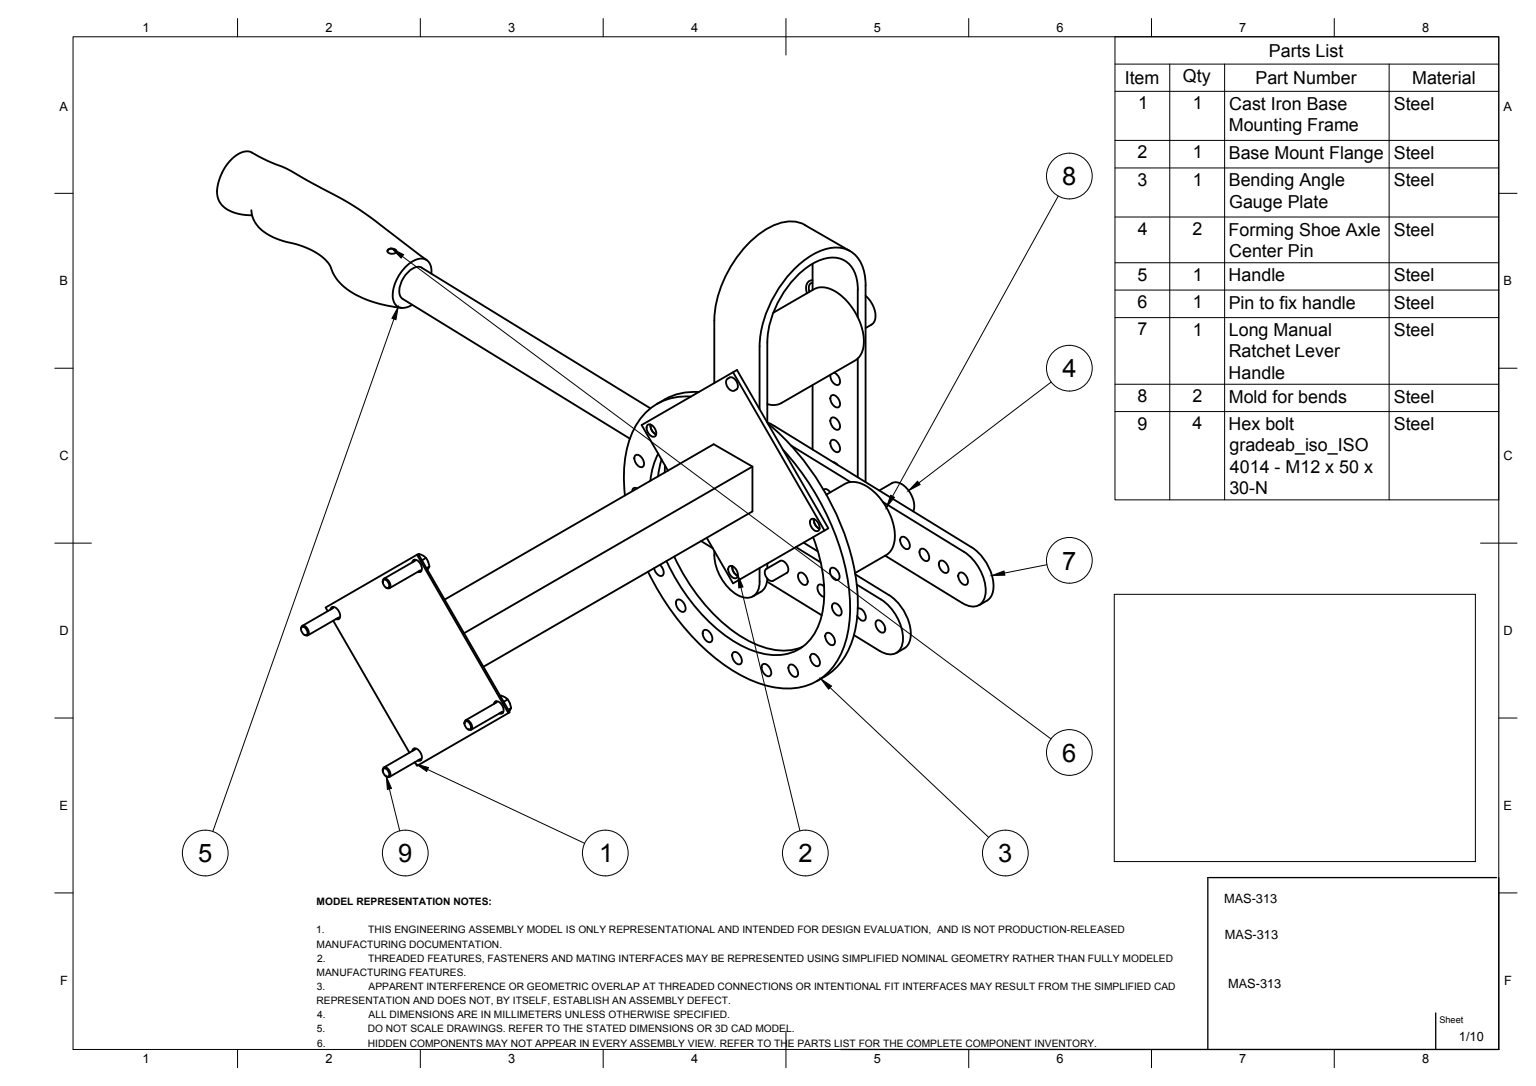
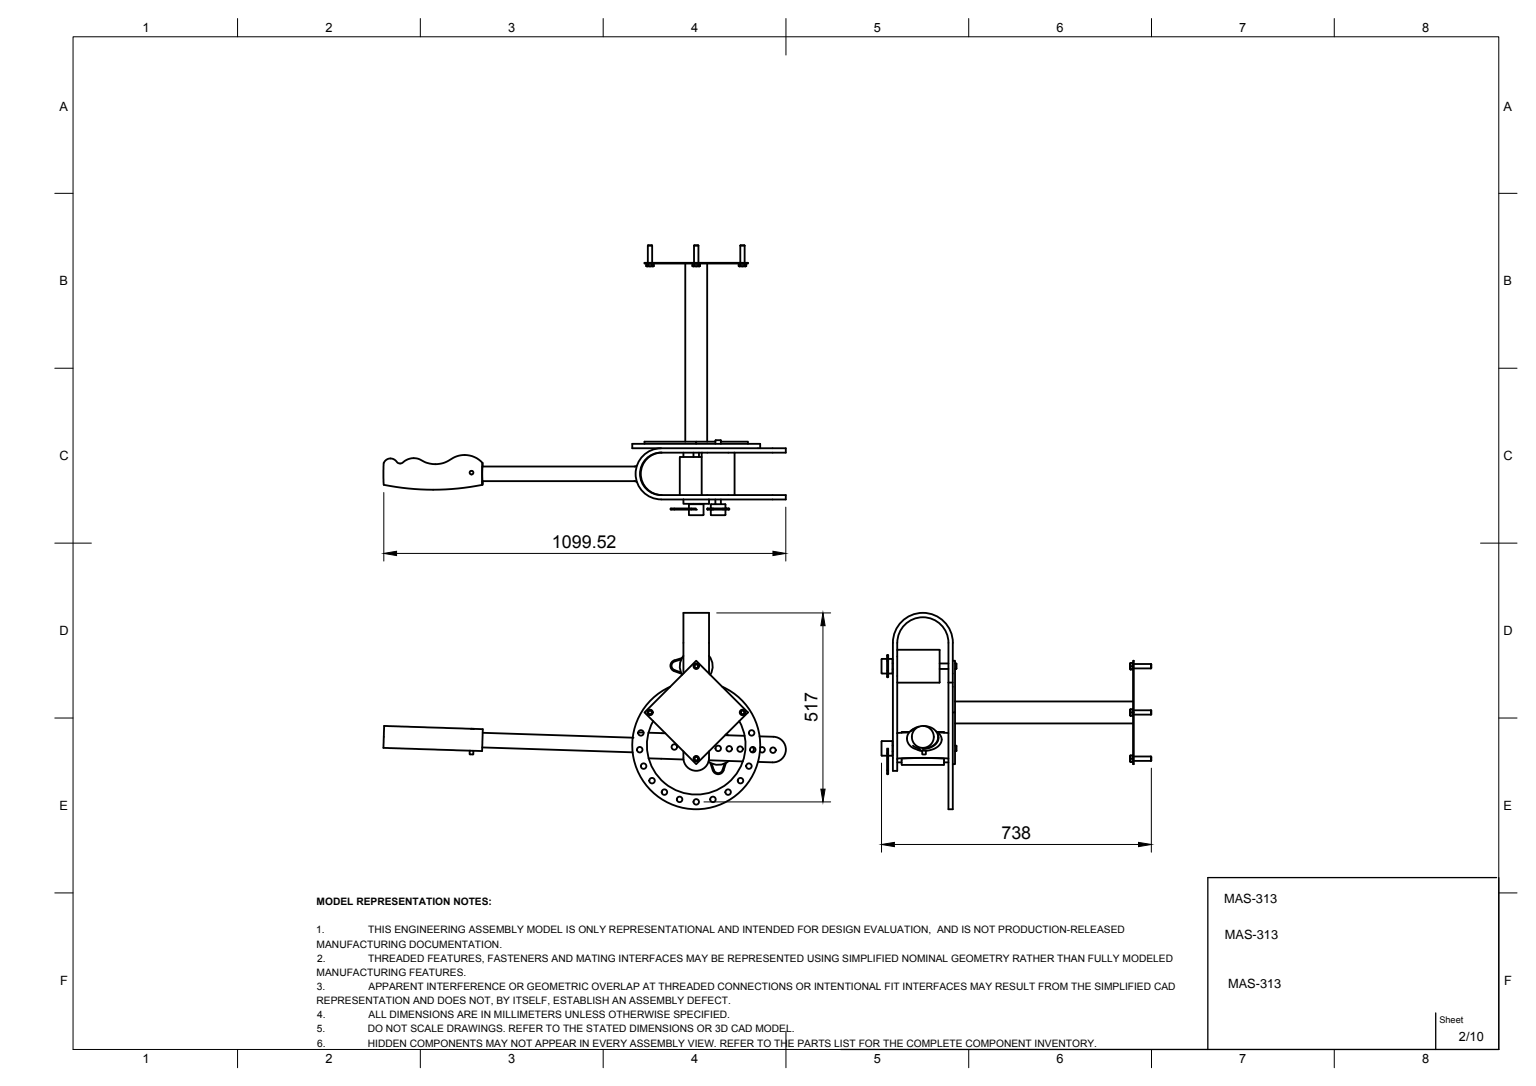
ISO-10303-21;
HEADER;
FILE_DESCRIPTION (('STEP AP214'),
    '1' );
FILE_NAME ('MAS-313',
    '2026-10-06T09:36:00',
    ( '' ),
    ( '' ),
    'SwSTEP 2.0',
    'SolidWorks 2025',
    '' );
FILE_SCHEMA (( 'AUTOMOTIVE_DESIGN' ));
ENDSEC;

DATA;
#1 = ORIENTED_EDGE ( 'NONE', *, *, #10134, .F. ) ;
#2 = ORIENTED_EDGE ( 'NONE', *, *, #7069, .T. ) ;
#3 = LINE ( 'NONE', #10333, #7200 ) ;
#4 = CARTESIAN_POINT ( 'NONE',  ( -828.8285638327245124, 78.34605190446923473, -105.0145692953451260 ) ) ;
#5 = EDGE_LOOP ( 'NONE', ( #11080, #1788 ) ) ;
#6 = CARTESIAN_POINT ( 'NONE',  ( -384.9774416452893888, 80.69083648313058177, -144.6406486762352870 ) ) ;
#7 = DIRECTION ( 'NONE',  ( 0.000000000000000000, 0.000000000000000000, 1.000000000000000000 ) ) ;
#8 = CARTESIAN_POINT ( 'NONE',  ( -374.9348459032029837, 78.20628728207141478, -105.0188168623670322 ) ) ;
#9 = CARTESIAN_POINT ( 'NONE',  ( -305.0000000000000568, 81.99999999999995737, -89.68077099980384048 ) ) ;
#10 = CIRCLE ( 'NONE', #8517, 8.500000000000007105 ) ;
#11 = EDGE_CURVE ( 'NONE', #3523, #3290, #9059, .T. ) ;
#12 = DIRECTION ( 'NONE',  ( -8.163404592832030268E-17, 1.000000000000000000, -0.000000000000000000 ) ) ;
#13 = CARTESIAN_POINT ( 'NONE',  ( -6.360897667028196044E-14, -494.9999999999998863, -141.4213562373094817 ) ) ;
#14 = EDGE_CURVE ( 'NONE', #10023, #7883, #9995, .T. ) ;
#15 = CARTESIAN_POINT ( 'NONE',  ( -795.0000000000070486, 70.44548139156158584, -96.78565065507937959 ) ) ;
#16 = CARTESIAN_POINT ( 'NONE',  ( -820.7717470982067880, 82.64484858469236883, -104.6903222377189593 ) ) ;
#17 = CYLINDRICAL_SURFACE ( 'NONE', #5203, 7.500000000000007105 ) ;
#18 = CIRCLE ( 'NONE', #8899, 134.9999999999999716 ) ;
#19 = CARTESIAN_POINT ( 'NONE',  ( -826.0529305544633871, 83.16438776978758085, -144.6472496521801929 ) ) ;
#20 = VERTEX_POINT ( 'NONE', #8026 ) ;
#21 = CARTESIAN_POINT ( 'NONE',  ( -824.1603064692799308, 83.67418067986842800, -144.6105757924095485 ) ) ;
#22 = ADVANCED_FACE ( 'NONE', ( #9876 ), #2276, .F. ) ;
#23 = SHAPE_DEFINITION_REPRESENTATION ( #9502, #690 ) ;
#24 = CARTESIAN_POINT ( 'NONE',  ( -374.1619648394964770, 92.84764663444484256, -97.33358173750130504 ) ) ;
#25 = ORIENTED_EDGE ( 'NONE', *, *, #6395, .T. ) ;
#26 = DIRECTION ( 'NONE',  ( 0.000000000000000000, 0.000000000000000000, 1.000000000000000000 ) ) ;
#27 = AXIS2_PLACEMENT_3D ( 'NONE', #9687, #6908, #2335 ) ;
#28 = CARTESIAN_POINT ( 'NONE',  ( -976.0610374937461984, 42.74778062430068104, -107.9061927053324155 ) ) ;
#29 = DIRECTION ( 'NONE',  ( 0.000000000000000000, 0.000000000000000000, 1.000000000000000000 ) ) ;
#30 = CARTESIAN_POINT ( 'NONE',  ( 19.97706055966621008, 179.9215598820742628, -126.1361639878079757 ) ) ;
#31 = CARTESIAN_POINT ( 'NONE',  ( 9.184850993605149917E-16, 0.000000000000000000, -133.9213562373095101 ) ) ;
#32 = TOROIDAL_SURFACE ( 'NONE', #418, 8.500000000000007105, 1.000000000000000000 ) ;
#33 = EDGE_CURVE ( 'NONE', #7221, #5849, #1766, .T. ) ;
#34 = ORIENTED_EDGE ( 'NONE', *, *, #7230, .T. ) ;
#35 = CARTESIAN_POINT ( 'NONE',  ( -374.8624431792070482, 77.47276654782569949, -154.2594059479313842 ) ) ;
#36 = CARTESIAN_POINT ( 'NONE',  ( -372.1683858186218004, 101.7385701426550071, -104.8071179324957569 ) ) ;
#37 = ORIENTED_EDGE ( 'NONE', *, *, #6606, .T. ) ;
#38 = CARTESIAN_POINT ( 'NONE',  ( -795.0000000000065938, 109.8950841424301217, -113.1262384684096105 ) ) ;
#39 = PRODUCT_RELATED_PRODUCT_CATEGORY ( 'part', '', ( #12175 ) ) ;
#40 = DIRECTION ( 'NONE',  ( -6.195440985631454085E-17, 0.000000000000000000, 1.000000000000000000 ) ) ;
#41 = CARTESIAN_POINT ( 'NONE',  ( -951.5459139781262365, 122.3346817490816676, -136.2353035311979852 ) ) ;
#42 = LINE ( 'NONE', #11363, #8844 ) ;
#43 = AXIS2_PLACEMENT_3D ( 'NONE', #1624, #5382, #1881 ) ;
#44 = CARTESIAN_POINT ( 'NONE',  ( -20.77482174596512010, 180.9926187296579201, -123.5402880645762451 ) ) ;
#45 = ORIENTED_EDGE ( 'NONE', *, *, #10615, .T. ) ;
#46 = DIRECTION ( 'NONE',  ( -0.7071067811865526798, 0.000000000000000000, 0.7071067811865423547 ) ) ;
#47 = EDGE_CURVE ( 'NONE', #6610, #12185, #4189, .T. ) ;
#48 = CARTESIAN_POINT ( 'NONE',  ( 7.653191805780027529E-16, 139.9999999999999716, -126.4213562373094959 ) ) ;
#49 = LINE ( 'NONE', #8712, #562 ) ;
#50 = CARTESIAN_POINT ( 'NONE',  ( -954.3284336448712111, 118.5422944683825932, -141.4553492942762318 ) ) ;
#51 = CARTESIAN_POINT ( 'NONE',  ( -379.1625717519825685, 101.9990905548760622, -123.9924296326342414 ) ) ;
#52 =( NAMED_UNIT ( * ) PLANE_ANGLE_UNIT ( ) SI_UNIT ( $, .RADIAN. ) );
#53 = DIRECTION ( 'NONE',  ( -8.163404592832030268E-17, 1.000000000000000000, -0.000000000000000000 ) ) ;
#54 = DIRECTION ( 'NONE',  ( -0.000000000000000000, 1.000000000000000000, 7.930164461608263644E-17 ) ) ;
#55 = ORIENTED_EDGE ( 'NONE', *, *, #5184, .F. ) ;
#56 = CARTESIAN_POINT ( 'NONE',  ( 1.561981751485805177E-12, 12.00000000000000000, 23.57864376269050410 ) ) ;
#57 = CARTESIAN_POINT ( 'NONE',  ( -370.6528479074003144, 106.2912024161782654, -136.2244394883228154 ) ) ;
#58 = ORIENTED_EDGE ( 'NONE', *, *, #10485, .F. ) ;
#59 = CARTESIAN_POINT ( 'NONE',  ( -1046.457602311632627, 98.67849639484583690, -149.7857175106632894 ) ) ;
#60 = CARTESIAN_POINT ( 'NONE',  ( -1054.407929976944160, 113.5897173251037628, -130.5712005305405228 ) ) ;
#61 = CIRCLE ( 'NONE', #6581, 7.500000000000007105 ) ;
#62 = FACE_BOUND ( 'NONE', #10137, .T. ) ;
#63 = ORIENTED_EDGE ( 'NONE', *, *, #11154, .T. ) ;
#64 = VERTEX_POINT ( 'NONE', #2451 ) ;
#65 = CARTESIAN_POINT ( 'NONE',  ( -365.0000000000000568, 81.99999999999997158, -124.6807709998038405 ) ) ;
#66 = CARTESIAN_POINT ( 'NONE',  ( -119.9999999999999858, 12.00000000000001421, -126.4213562373086575 ) ) ;
#67 = CARTESIAN_POINT ( 'NONE',  ( -1027.708477481189902, 65.70736702952426356, -149.7857175106639431 ) ) ;
#68 = EDGE_CURVE ( 'NONE', #11346, #11763, #11644, .T. ) ;
#69 = VERTEX_POINT ( 'NONE', #7089 ) ;
#70 = CARTESIAN_POINT ( 'NONE',  ( -384.9468357058332799, 80.02786880483864707, -144.5860799529720566 ) ) ;
#71 = CARTESIAN_POINT ( 'NONE',  ( 6.899999999999999467, -7.794228634059934713, 4.500000000000015987 ) ) ;
#72 = CARTESIAN_POINT ( 'NONE',  ( -374.8121035591796044, 76.80383275076532357, -95.25780428797004618 ) ) ;
#73 = LINE ( 'NONE', #6513, #3701 ) ;
#74 = AXIS2_PLACEMENT_3D ( 'NONE', #9091, #4403, #8176 ) ;
#75 = EDGE_LOOP ( 'NONE', ( #6909, #2744, #1662, #2481 ) ) ;
#76 = AXIS2_PLACEMENT_3D ( 'NONE', #1140, #8678, #11512 ) ;
#77 = DIRECTION ( 'NONE',  ( 0.000000000000000000, 0.000000000000000000, 1.000000000000000000 ) ) ;
#78 = CARTESIAN_POINT ( 'NONE',  ( 19.99739293773369653, 178.7258229095291426, -125.0390604444466902 ) ) ;
#79 = CARTESIAN_POINT ( 'NONE',  ( -1062.665377791213132, 57.01990411978262330, -103.3307627799634503 ) ) ;
#80 = CARTESIAN_POINT ( 'NONE',  ( -97.49999999999998579, 24.00000000000001421, -126.4213562373088564 ) ) ;
#81 = LINE ( 'NONE', #4059, #683 ) ;
#82 = CARTESIAN_POINT ( 'NONE',  ( -1032.658196452833636, 44.72920460984212809, -126.6442663926291914 ) ) ;
#83 = VERTEX_POINT ( 'NONE', #3428 ) ;
#84 = CARTESIAN_POINT ( 'NONE',  ( -384.0214413967224800, 73.66668219692796526, -106.4901515991773522 ) ) ;
#85 = ORIENTED_EDGE ( 'NONE', *, *, #1558, .T. ) ;
#86 = EDGE_CURVE ( 'NONE', #586, #9244, #5121, .T. ) ;
#87 = VECTOR ( 'NONE', #10625, 1000.000000000000000 ) ;
#88 = APPLICATION_PROTOCOL_DEFINITION ( 'draft international standard', 'automotive_design', 1998, #7796 ) ;
#89 = AXIS2_PLACEMENT_3D ( 'NONE', #10782, #5094, #8125 ) ;
#90 = VERTEX_POINT ( 'NONE', #4259 ) ;
#91 = CARTESIAN_POINT ( 'NONE',  ( -953.8433812051914629, 65.95343150956773570, -99.57582448894520155 ) ) ;
#92 = LINE ( 'NONE', #10358, #965 ) ;
#93 = EDGE_CURVE ( 'NONE', #7054, #9028, #4139, .T. ) ;
#94 = CYLINDRICAL_SURFACE ( 'NONE', #4643, 70.00000000000002842 ) ;
#95 = PRODUCT_DEFINITION_CONTEXT ( 'detailed design', #1716, 'design' ) ;
#96 = VECTOR ( 'NONE', #2050, 1000.000000000000000 ) ;
#97 = AXIS2_PLACEMENT_3D ( 'NONE', #11633, #3261, #1306 ) ;
#98 = CARTESIAN_POINT ( 'NONE',  ( -1054.691024341069351, 108.1159421897237110, -107.9061927053325149 ) ) ;
#99 = FACE_OUTER_BOUND ( 'NONE', #2484, .T. ) ;
#100 = CARTESIAN_POINT ( 'NONE',  ( -19.99217429592516737, 178.8549194765174946, -125.3522826812394584 ) ) ;
#101 = ORIENTED_EDGE ( 'NONE', *, *, #4439, .T. ) ;
#102 = CARTESIAN_POINT ( 'NONE',  ( -383.2436296729866285, 93.11778785828077787, -108.0524282450768681 ) ) ;
#103 = ORIENTED_EDGE ( 'NONE', *, *, #874, .T. ) ;
#105 = EDGE_CURVE ( 'NONE', #546, #9394, #11040, .T. ) ;
#104 = CARTESIAN_POINT ( 'NONE',  ( -1054.519145619997744, 111.4921997120089401, -113.1262384684101079 ) ) ;
#106 = CARTESIAN_POINT ( 'NONE',  ( 0.09252763182291999511, -8.674330214978049014, -2.975619346028157697 ) ) ;
#107 = CARTESIAN_POINT ( 'NONE',  ( -1024.848917040341576, 116.4131098345822437, -136.2353035311980420 ) ) ;
#108 = CARTESIAN_POINT ( 'NONE',  ( 19.97032670689476674, 177.8811654734197134, -125.7875625598146883 ) ) ;
#109 = CARTESIAN_POINT ( 'NONE',  ( -1045.884592419585942, 115.0579440276405450, -118.7903414690682524 ) ) ;
#110 = ORIENTED_EDGE ( 'NONE', *, *, #8930, .F. ) ;
#111 = DIRECTION ( 'NONE',  ( -8.163404592832030268E-17, 1.000000000000000000, -0.000000000000000000 ) ) ;
#112 = DIRECTION ( 'NONE',  ( 1.000000000000000000, 0.000000000000000000, 0.000000000000000000 ) ) ;
#113 = CARTESIAN_POINT ( 'NONE',  ( -954.7734463792789938, 107.7731650919854758, -149.7857175106632042 ) ) ;
#114 = LINE ( 'NONE', #2966, #2548 ) ;
#115 = DIRECTION ( 'NONE',  ( 0.000000000000000000, 1.000000000000000000, 0.000000000000000000 ) ) ;
#116 = ORIENTED_EDGE ( 'NONE', *, *, #6003, .T. ) ;
#117 = CYLINDRICAL_SURFACE ( 'NONE', #9034, 7.500000000000007105 ) ;
#118 = PRODUCT ( 'Base Mount Flange', 'Base Mount Flange', '', ( #4909 ) ) ;
#119 = CARTESIAN_POINT ( 'NONE',  ( -1065.000000000006366, 107.1049510380562850, -141.4553492942759192 ) ) ;
#120 = EDGE_CURVE ( 'NONE', #2594, #3971, #5709, .T. ) ;
#121 = EDGE_CURVE ( 'NONE', #609, #1988, #8932, .T. ) ;
#122 = ORIENTED_EDGE ( 'NONE', *, *, #10751, .T. ) ;
#123 = FACE_BOUND ( 'NONE', #7167, .T. ) ;
#124 = ORIENTED_EDGE ( 'NONE', *, *, #7991, .T. ) ;
#125 = VERTEX_POINT ( 'NONE', #4313 ) ;
#126 = CARTESIAN_POINT ( 'NONE',  ( 19.97657209060318806, 179.2792238463859746, -123.5006916350263282 ) ) ;
#127 = CARTESIAN_POINT ( 'NONE',  ( -21.00467209899894172, 181.7165653707129422, -124.9111601018296795 ) ) ;
#128 = FACE_BOUND ( 'NONE', #2869, .T. ) ;
#129 = CARTESIAN_POINT ( 'NONE',  ( -956.7203770923184720, 58.97922774997713447, -146.0307792196449839 ) ) ;
#130 = CARTESIAN_POINT ( 'NONE',  ( -383.8870708247850985, 73.11411249519194655, -142.6104777306848916 ) ) ;
#131 = CARTESIAN_POINT ( 'NONE',  ( -120.8820948793972434, 12.00000000000000000, -179.1989091883324363 ) ) ;
#132 = CARTESIAN_POINT ( 'NONE',  ( -384.9021618238296583, 79.34260306531722051, -104.8553288783483453 ) ) ;
#133 = VECTOR ( 'NONE', #10097, 1000.000000000000000 ) ;
#134 = CARTESIAN_POINT ( 'NONE',  ( 1.387778780781445676E-14, -58.00000000000000711, 126.4213562373094959 ) ) ;
#135 = ORIENTED_EDGE ( 'NONE', *, *, #8137, .F. ) ;
#136 = AXIS2_PLACEMENT_3D ( 'NONE', #2557, #579, #5269 ) ;
#137 = CARTESIAN_POINT ( 'NONE',  ( -818.1708872189576596, 40.82851623284144438, -103.3307627799635640 ) ) ;
#138 = CARTESIAN_POINT ( 'NONE',  ( -823.5000624989293101, 83.67424195610622917, -104.7509713550767287 ) ) ;
#139 = CARTESIAN_POINT ( 'NONE',  ( -901.8967518049312275, 57.00804855647886171, -130.5712005305400965 ) ) ;
#140 = VERTEX_POINT ( 'NONE', #3194 ) ;
#141 = CARTESIAN_POINT ( 'NONE',  ( -385.0078061158059768, 82.93686821115872476, -104.6668923901645769 ) ) ;
#142 = CARTESIAN_POINT ( 'NONE',  ( -825.4378685752795946, 73.92905737501402541, -154.6600603160834169 ) ) ;
#143 = EDGE_LOOP ( 'NONE', ( #3113, #5997, #4149, #12106, #10278, #5170, #6052 ) ) ;
#144 = SHAPE_DEFINITION_REPRESENTATION ( #1806, #1102 ) ;
#145 = ORIENTED_EDGE ( 'NONE', *, *, #5842, .F. ) ;
#146 = CARTESIAN_POINT ( 'NONE',  ( -1021.607260580486013, 54.24386729702176524, -118.7903414690683661 ) ) ;
#147 = VECTOR ( 'NONE', #6691, 1000.000000000000000 ) ;
#148 = DIRECTION ( 'NONE',  ( 0.000000000000000000, 0.000000000000000000, -1.000000000000000000 ) ) ;
#149 = FACE_OUTER_BOUND ( 'NONE', #6887, .T. ) ;
#150 = CIRCLE ( 'NONE', #8476, 7.500000000000007105 ) ;
#151 = CARTESIAN_POINT ( 'NONE',  ( -19.98114923013653765, 179.3963068953591176, -125.9321215961336975 ) ) ;
#152 = ORIENTED_EDGE ( 'NONE', *, *, #2859, .F. ) ;
#153 = CARTESIAN_POINT ( 'NONE',  ( -374.9443013845391874, 79.15238586648754904, -154.5107090977903113 ) ) ;
#154 = VERTEX_POINT ( 'NONE', #2390 ) ;
#155 = CARTESIAN_POINT ( 'NONE',  ( -954.3284336448667773, 118.5422944683823800, -107.9061927053323302 ) ) ;
#156 = AXIS2_PLACEMENT_3D ( 'NONE', #6549, #9206, #9335 ) ;
#157 = FACE_OUTER_BOUND ( 'NONE', #4978, .T. ) ;
#158 = CARTESIAN_POINT ( 'NONE',  ( -1054.519145619990923, 111.4921997120091106, -136.2353035311978999 ) ) ;
#159 = DIRECTION ( 'NONE',  ( -1.186840563529527301E-16, 1.000000000000000000, -0.000000000000000000 ) ) ;
#160 = AXIS2_PLACEMENT_3D ( 'NONE', #10271, #8167, #6559 ) ;
#161 = EDGE_CURVE ( 'NONE', #6627, #7697, #6700, .T. ) ;
#162 = CARTESIAN_POINT ( 'NONE',  ( -20.82968904857387216, 181.3053215700974192, -123.7910769712144798 ) ) ;
#163 = ORIENTED_EDGE ( 'NONE', *, *, #8870, .T. ) ;
#164 = CARTESIAN_POINT ( 'NONE',  ( -150.0000000000000000, -9.213203435596451385, -126.4213562373084301 ) ) ;
#165 = EDGE_CURVE ( 'NONE', #7498, #4712, #7501, .T. ) ;
#166 = AXIS2_PLACEMENT_3D ( 'NONE', #11994, #9209, #3384 ) ;
#167 = DIRECTION ( 'NONE',  ( 1.000000000000000000, -1.876626137810916309E-30, 2.081668171172161734E-17 ) ) ;
#168 = CYLINDRICAL_SURFACE ( 'NONE', #6692, 7.500000000000007105 ) ;
#169 = CARTESIAN_POINT ( 'NONE',  ( -852.9318753287220716, 113.3383058689776277, -141.4553492942764024 ) ) ;
#170 = CARTESIAN_POINT ( 'NONE',  ( -371.2169330467067994, 104.7056300760318379, -109.5948443055706036 ) ) ;
#171 = CARTESIAN_POINT ( 'NONE',  ( -126.4213562373094959, -492.9999999999998863, 2.255140518769849223E-14 ) ) ;
#172 = CARTESIAN_POINT ( 'NONE',  ( 1.414009460465297036E-14, -9.213203435596451385, -126.4213562373094959 ) ) ;
#173 = ORIENTED_EDGE ( 'NONE', *, *, #11290, .T. ) ;
#174 = CARTESIAN_POINT ( 'NONE',  ( -240.0000000000000000, 151.9999999999999716, -126.4213562373078190 ) ) ;
#175 = VECTOR ( 'NONE', #6548, 1000.000000000000000 ) ;
#176 = AXIS2_PLACEMENT_3D ( 'NONE', #10566, #11560, #2167 ) ;
#177 = FACE_BOUND ( 'NONE', #6264, .T. ) ;
#178 = VERTEX_POINT ( 'NONE', #3366 ) ;
#179 = ORIENTED_EDGE ( 'NONE', *, *, #161, .T. ) ;
#180 = CYLINDRICAL_SURFACE ( 'NONE', #1475, 20.00000000000004619 ) ;
#181 = CARTESIAN_POINT ( 'NONE',  ( -380.7070114274824846, 99.23877955377430737, -134.8374997946181111 ) ) ;
#182 = CARTESIAN_POINT ( 'NONE',  ( -956.4793285278399253, 64.87563161486532692, -149.7857175106635452 ) ) ;
#183 = EDGE_LOOP ( 'NONE', ( #1625, #2228, #7810, #4343, #5772, #11900, #7059 ) ) ;
#184 = ADVANCED_FACE ( 'NONE', ( #596 ), #4371, .T. ) ;
#185 = CARTESIAN_POINT ( 'NONE',  ( -384.7087986609971608, 86.59177257609081835, -144.1578396759514646 ) ) ;
#186 = CARTESIAN_POINT ( 'NONE',  ( 1.874378101782966050E-12, -6.000000000000006217, 61.07864376269051121 ) ) ;
#187 = CARTESIAN_POINT ( 'NONE',  ( -382.1259332444888628, 67.82440028630135487, -110.5571689112878033 ) ) ;
#188 = CARTESIAN_POINT ( 'NONE',  ( 0.000000000000000000, 0.000000000000000000, 0.000000000000000000 ) ) ;
#189 = ORIENTED_EDGE ( 'NONE', *, *, #1792, .T. ) ;
#190 = CARTESIAN_POINT ( 'NONE',  ( -954.4431216459919369, 51.77564274757662588, -136.2353035311985820 ) ) ;
#191 = PRODUCT_DEFINITION ( 'UNKNOWN', '', #10585, #95 ) ;
#192 = VERTEX_POINT ( 'NONE', #5981 ) ;
#193 = ORIENTED_EDGE ( 'NONE', *, *, #8592, .F. ) ;
#194 = CARTESIAN_POINT ( 'NONE',  ( -817.4144546772188278, 30.82543593413045713, -113.1262384684093689 ) ) ;
#195 = CARTESIAN_POINT ( 'NONE',  ( -822.2163178171820164, 83.41010758653678181, -104.7304854148475499 ) ) ;
#196 = LINE ( 'NONE', #11401, #4433 ) ;
#197 = EDGE_LOOP ( 'NONE', ( #6499, #7897, #12076, #5197 ) ) ;
#198 =( REPRESENTATION_RELATIONSHIP ('NONE','NONE', #12149, #4488 ) REPRESENTATION_RELATIONSHIP_WITH_TRANSFORMATION ( #4114 )SHAPE_REPRESENTATION_RELATIONSHIP( ) );
#199 = EDGE_CURVE ( 'NONE', #11915, #1856, #8826, .T. ) ;
#200 = CARTESIAN_POINT ( 'NONE',  ( -384.9575332945760806, 80.23676698716798228, -104.7563694268733059 ) ) ;
#201 = ORIENTED_EDGE ( 'NONE', *, *, #5756, .F. ) ;
#202 = CARTESIAN_POINT ( 'NONE',  ( -828.1602791247941013, 76.17169011767150266, -154.6744596958750151 ) ) ;
#203 = ORIENTED_EDGE ( 'NONE', *, *, #874, .F. ) ;
#204 = CARTESIAN_POINT ( 'NONE',  ( -305.0000000000000568, 11.99999999999998224, -89.68077099980384048 ) ) ;
#205 = APPLICATION_PROTOCOL_DEFINITION ( 'draft international standard', 'automotive_design', 1998, #366 ) ;
#206 = VERTEX_POINT ( 'NONE', #8210 ) ;
#207 = CARTESIAN_POINT ( 'NONE',  ( -1048.438004920983758, 39.66697241395321782, -122.7172756069793138 ) ) ;
#208 = DIRECTION ( 'NONE',  ( -0.000000000000000000, 1.000000000000000000, 7.930164461608263644E-17 ) ) ;
#209 = CARTESIAN_POINT ( 'NONE',  ( 0.1482032042081581624, 2.204400401829194056, -9.000000000000001776 ) ) ;
#210 = DIRECTION ( 'NONE',  ( 3.061276722312011504E-17, -1.000000000000000000, 0.000000000000000000 ) ) ;
#211 = CARTESIAN_POINT ( 'NONE',  ( -240.0000000000000000, 24.00000000000000711, -126.4213562373078190 ) ) ;
#212 = UNCERTAINTY_MEASURE_WITH_UNIT (LENGTH_MEASURE( 1.000000000000000082E-05 ), #7205, 'distance_accuracy_value', 'NONE');
#213 = VECTOR ( 'NONE', #11605, 1000.000000000000000 ) ;
#214 = CARTESIAN_POINT ( 'NONE',  ( -951.5459139781289650, 122.3346817490815681, -113.1262384684093263 ) ) ;
#215 = DIRECTION ( 'NONE',  ( -0.000000000000000000, 1.000000000000000000, 7.930164461608263644E-17 ) ) ;
#216 = DIRECTION ( 'NONE',  ( 0.000000000000000000, 0.000000000000000000, 1.000000000000000000 ) ) ;
#217 = ORIENTED_EDGE ( 'NONE', *, *, #11458, .T. ) ;
#218 = EDGE_LOOP ( 'NONE', ( #11467, #11457 ) ) ;
#219 = CARTESIAN_POINT ( 'NONE',  ( -1061.673215548682720, 86.58918783539685649, -95.06748246948023962 ) ) ;
#220 = CARTESIAN_POINT ( 'NONE',  ( -954.0688428831344936, 124.4732772249357282, -130.5712005305405796 ) ) ;
#221 = DIRECTION ( 'NONE',  ( -1.000000000000000000, 0.000000000000000000, 0.000000000000000000 ) ) ;
#222 = CARTESIAN_POINT ( 'NONE',  ( 19.92179295512113057, 178.7027072646551744, -122.9085123094865537 ) ) ;
#223 = CIRCLE ( 'NONE', #7140, 7.500000000000007105 ) ;
#224 = LINE ( 'NONE', #2033, #3608 ) ;
#225 = EDGE_LOOP ( 'NONE', ( #261, #5060, #2254, #7295, #1076, #408 ) ) ;
#226 = CYLINDRICAL_SURFACE ( 'NONE', #5194, 7.500000000000007105 ) ;
#227 = CARTESIAN_POINT ( 'NONE',  ( -820.5194676126008062, 82.43685310047841597, -104.6842045117117266 ) ) ;
#228 = CARTESIAN_POINT ( 'NONE',  ( 0.000000000000000000, -494.9999999999998863, 0.000000000000000000 ) ) ;
#229 = CARTESIAN_POINT ( 'NONE',  ( -1025.044148074459827, 113.2108726315406813, -141.4553492942762318 ) ) ;
#230 =( LENGTH_UNIT ( ) NAMED_UNIT ( * ) SI_UNIT ( .MILLI., .METRE. ) );
#231 = CARTESIAN_POINT ( 'NONE',  ( 120.8820948793965186, 0.000000000000000000, -194.1989091883332890 ) ) ;
#232 = FACE_BOUND ( 'NONE', #2861, .T. ) ;
#233 = VERTEX_POINT ( 'NONE', #6533 ) ;
#234 = CARTESIAN_POINT ( 'NONE',  ( -1010.922847972424620, 120.6260792194949829, -126.6442663926288503 ) ) ;
#235 = EDGE_CURVE ( 'NONE', #11998, #11124, #7336, .T. ) ;
#236 = DIRECTION ( 'NONE',  ( -0.000000000000000000, -1.000000000000000000, -1.757987137413040192E-14 ) ) ;
#237 = CARTESIAN_POINT ( 'NONE',  ( -853.1108559448500728, 99.60875591605696400, -149.7857175106632610 ) ) ;
#238 = EDGE_CURVE ( 'NONE', #2268, #7247, #10053, .T. ) ;
#239 = CARTESIAN_POINT ( 'NONE',  ( 0.000000000000000000, 0.000000000000000000, -89.68077099980401101 ) ) ;
#240 = ORIENTED_EDGE ( 'NONE', *, *, #4269, .F. ) ;
#241 = ORIENTED_EDGE ( 'NONE', *, *, #8867, .F. ) ;
#242 = CIRCLE ( 'NONE', #10114, 7.500000000000020428 ) ;
#243 = CARTESIAN_POINT ( 'NONE',  ( -383.7609474437092558, 91.40550212013970111, -142.3698073093449636 ) ) ;
#244 = CARTESIAN_POINT ( 'NONE',  ( 3.123963502971610252E-13, 12.00000000000000000, -96.42135623730949590 ) ) ;
#245 = CARTESIAN_POINT ( 'NONE',  ( -956.2104666674752025, 71.56905446038098262, -152.5758913445294809 ) ) ;
#246 = DIRECTION ( 'NONE',  ( 0.000000000000000000, 0.000000000000000000, -1.000000000000000000 ) ) ;
#247 = CARTESIAN_POINT ( 'NONE',  ( -384.0991065115986771, 74.01283611578425337, -143.0196247845297819 ) ) ;
#248 = FACE_OUTER_BOUND ( 'NONE', #11895, .T. ) ;
#249 = AXIS2_PLACEMENT_3D ( 'NONE', #6784, #11489, #10438 ) ;
#250 = EDGE_LOOP ( 'NONE', ( #6658, #11800 ) ) ;
#251 = CARTESIAN_POINT ( 'NONE',  ( -795.0000000000020464, 52.38665522077208436, -130.5712005305402670 ) ) ;
#252 = ORIENTED_EDGE ( 'NONE', *, *, #941, .T. ) ;
#253 = EDGE_CURVE ( 'NONE', #7231, #4288, #5520, .T. ) ;
#254 = FACE_OUTER_BOUND ( 'NONE', #3985, .T. ) ;
#255 = CARTESIAN_POINT ( 'NONE',  ( 20.99826841500651753, 178.6919330321067036, -124.8534679218782770 ) ) ;
#256 = VECTOR ( 'NONE', #4482, 1000.000000000000000 ) ;
#257 = CARTESIAN_POINT ( 'NONE',  ( -1014.004070199759440, 54.58258344709550869, -113.1262384684095537 ) ) ;
#258 = LINE ( 'NONE', #2469, #6072 ) ;
#259 = CARTESIAN_POINT ( 'NONE',  ( -1014.004070199769671, 54.58258344709567922, -136.2353035311988947 ) ) ;
#260 = EDGE_LOOP ( 'NONE', ( #3241, #8071, #5792, #1069 ) ) ;
#261 = ORIENTED_EDGE ( 'NONE', *, *, #5093, .F. ) ;
#262 = DIRECTION ( 'NONE',  ( 1.186840563529527301E-16, -1.000000000000000000, 0.000000000000000000 ) ) ;
#263 = ORIENTED_EDGE ( 'NONE', *, *, #5400, .T. ) ;
#264 = ORIENTED_EDGE ( 'NONE', *, *, #2535, .T. ) ;
#265 = CARTESIAN_POINT ( 'NONE',  ( -976.2351830775012331, 35.86345807843999012, -118.7903414690679824 ) ) ;
#266 = VECTOR ( 'NONE', #3751, 1000.000000000000000 ) ;
#267 = CIRCLE ( 'NONE', #6597, 5.035999999999999588 ) ;
#268 = CARTESIAN_POINT ( 'NONE',  ( -35.00000000000000000, 81.99999999999998579, 190.3192290001959748 ) ) ;
#269 = DIRECTION ( 'NONE',  ( 0.000000000000000000, 0.000000000000000000, -1.000000000000000000 ) ) ;
#270 = ADVANCED_FACE ( 'NONE', ( #2701 ), #10246, .F. ) ;
#271 = ADVANCED_FACE ( 'NONE', ( #9188 ), #1781, .F. ) ;
#272 = CARTESIAN_POINT ( 'NONE',  ( -1031.197907781702725, 107.2697845108577894, -103.3307627799635640 ) ) ;
#273 = DIRECTION ( 'NONE',  ( -0.000000000000000000, -0.000000000000000000, -1.000000000000000000 ) ) ;
#274 = CARTESIAN_POINT ( 'NONE',  ( -21.06063637301984670, 178.9270029669538360, -125.6999331669520501 ) ) ;
#275 = CIRCLE ( 'NONE', #3413, 1.000000000000001110 ) ;
#276 = VECTOR ( 'NONE', #8146, 1000.000000000000000 ) ;
#277 = ORIENTED_EDGE ( 'NONE', *, *, #5385, .T. ) ;
#278 = CIRCLE ( 'NONE', #3844, 7.500000000000013323 ) ;
#279 = DIRECTION ( 'NONE',  ( 1.000000000000000000, -1.262554838833776231E-16, 0.000000000000000000 ) ) ;
#280 = PRESENTATION_STYLE_ASSIGNMENT (( #11725 ) ) ;
#281 = ORIENTED_EDGE ( 'NONE', *, *, #1146, .T. ) ;
#282 = CARTESIAN_POINT ( 'NONE',  ( -853.3345817150102448, 81.97571759610518427, -95.06748246948041015 ) ) ;
#283 = EDGE_LOOP ( 'NONE', ( #6385, #2027 ) ) ;
#284 = CARTESIAN_POINT ( 'NONE',  ( -823.5047064235034213, 114.4566975831562274, -136.2353035311979284 ) ) ;
#285 = CARTESIAN_POINT ( 'NONE',  ( -6.106226635438360972E-13, 0.000000000000000000, -244.6807709998039400 ) ) ;
#286 =( BOUNDED_SURFACE ( )  B_SPLINE_SURFACE ( 3, 2, ( 
 ( #5085, #8801, #7187 ),
 ( #2485, #10957, #1263 ),
 ( #8857, #5024, #11650 ),
 ( #3170, #3727, #4408 ),
 ( #11016, #2547, #5517 ),
 ( #8178, #6322, #5324 ),
 ( #7317, #11945, #8318 ),
 ( #10089, #8249, #6509 ),
 ( #10030, #9093, #12007 ),
 ( #1688, #3526, #11218 ),
 ( #7251, #4472, #11082 ),
 ( #5581, #9355, #1623 ),
 ( #9160, #4606, #10151 ),
 ( #5381, #7377, #6262 ),
 ( #2741, #696, #632 ),
 ( #2607, #12145, #10219 ),
 ( #3462, #6382, #1561 ),
 ( #4667, #11150, #5445 ),
 ( #8445, #833, #9293 ),
 ( #9226, #767, #1818 ),
 ( #10279, #4542, #12077 ),
 ( #3587, #2673, #8382 ),
 ( #6448, #1756, #3659 ),
 ( #12203, #7433, #7499 ),
 ( #11272, #899, #10395 ),
 ( #1013, #1880, #10338 ),
 ( #9532, #6744, #8677 ),
 ( #2057, #5700, #5878 ),
 ( #7805, #8611, #130 ),
 ( #6810, #3848, #247 ),
 ( #5644, #3967, #9417 ),
 ( #1077, #4724, #2801 ),
 ( #8500, #5755, #10464 ),
 ( #4780, #6573, #7557 ),
 ( #9594, #5816, #8551 ),
 ( #2982, #6688, #4890 ),
 ( #953, #2119, #70 ),
 ( #1999, #7621, #6 ),
 ( #8730, #4035, #11511 ),
 ( #3782, #3908, #1938 ),
 ( #4834, #1139, #9657 ),
 ( #11329, #7682, #11389 ),
 ( #2928, #10521, #2870 ),
 ( #6630, #11451, #1198 ),
 ( #7737, #9474, #185 ),
 ( #10581, #3039, #4953 ),
 ( #11376, #2915, #12133 ),
 ( #2729, #1924, #3713 ),
 ( #5746, #7490, #5685 ),
 ( #6437, #6677, #10272 ),
 ( #11264, #5568, #10208 ),
 ( #9521, #1746, #2791 ),
 ( #8368, #11315, #11205 ),
 ( #3646, #5508, #1066 ),
 ( #9283, #5631, #1805 ),
 ( #6561, #1501, #821 ),
 ( #6498, #10325, #12064 ),
 ( #4766, #9405, #2854 ),
 ( #7611, #4713, #3773 ),
 ( #6620, #999, #8541 ),
 ( #57, #3836, #398 ),
 ( #9872, #8599, #11437 ) ),
 .UNSPECIFIED., .F., .F., .F. ) 
 B_SPLINE_SURFACE_WITH_KNOTS ( ( 4, 2, 2, 2, 2, 2, 2, 2, 2, 2, 2, 2, 2, 2, 2, 2, 2, 2, 2, 2, 2, 2, 2, 2, 2, 2, 2, 2, 2, 2, 4 ),
 ( 3, 3 ),
 ( 0.09449389133479987879, 0.1003997595432298551, 0.1063056277516598314, 0.1092585618558748195, 0.1107350289079823136, 0.1122114959600898076, 0.1181173641685197701, 0.1195938312206272502, 0.1210702982727347443, 0.1240232323769497325, 0.1269761664811647206, 0.1284526335332722147, 0.1299291005853797087, 0.1358349687938096850, 0.1387879028980246732, 0.1402643699501321672, 0.1417408370022396613, 0.1476467052106696376, 0.1491231722627771317, 0.1505996393148846257, 0.1535525734190996139, 0.1565055075233146020, 0.1594584416275295902, 0.1653643098359595387, 0.1683172439401744991, 0.1697937109922819932, 0.1712701780443894872, 0.1771760462528194635, 0.1801289803570344517, 0.1830819144612494398, 0.1889877826696794161 ),
 ( 0.000000000000000000, 1.000000000000000000 ),
 .UNSPECIFIED. ) 
 GEOMETRIC_REPRESENTATION_ITEM ( )  RATIONAL_B_SPLINE_SURFACE ( (
 ( 1.000000000000000000, 0.8172789612915526414, 1.000000000000000000),
 ( 1.000000000000000000, 0.8218272198189814359, 1.000000000000000000),
 ( 1.000000000000000000, 0.8252177520338900285, 1.000000000000000000),
 ( 1.000000000000000000, 0.8291640623197805704, 1.000000000000000000),
 ( 1.000000000000000000, 0.8296443862460527452, 1.000000000000000000),
 ( 1.000000000000000000, 0.8281763619574273871, 1.000000000000000000),
 ( 1.000000000000000000, 0.8273214979613470188, 1.000000000000000000),
 ( 1.000000000000000000, 0.8254906886306150327, 1.000000000000000000),
 ( 1.000000000000000000, 0.8247876722294519292, 1.000000000000000000),
 ( 1.000000000000000000, 0.8232192861295574149, 1.000000000000000000),
 ( 1.000000000000000000, 0.8223523569020266821, 1.000000000000000000),
 ( 1.000000000000000000, 0.8176244427683647675, 1.000000000000000000),
 ( 1.000000000000000000, 0.8125861978211987857, 1.000000000000000000),
 ( 1.000000000000000000, 0.8050068216217169947, 1.000000000000000000),
 ( 1.000000000000000000, 0.8034229420457332793, 1.000000000000000000),
 ( 1.000000000000000000, 0.8001526181735703069, 1.000000000000000000),
 ( 1.000000000000000000, 0.7984703186739749992, 1.000000000000000000),
 ( 1.000000000000000000, 0.7932997541396797914, 1.000000000000000000),
 ( 1.000000000000000000, 0.7896878191176920359, 1.000000000000000000),
 ( 1.000000000000000000, 0.7822263873999749650, 1.000000000000000000),
 ( 1.000000000000000000, 0.7783766572002538409, 1.000000000000000000),
 ( 1.000000000000000000, 0.7724948447777896243, 1.000000000000000000),
 ( 1.000000000000000000, 0.7705164146871855690, 1.000000000000000000),
 ( 1.000000000000000000, 0.7665366243600161278, 1.000000000000000000),
 ( 1.000000000000000000, 0.7645334732995007210, 1.000000000000000000),
 ( 1.000000000000000000, 0.7545994289160806723, 1.000000000000000000),
 ( 1.000000000000000000, 0.7468282588146691880, 1.000000000000000000),
 ( 1.000000000000000000, 0.7361158826353683127, 1.000000000000000000),
 ( 1.000000000000000000, 0.7327031703348744207, 1.000000000000000000),
 ( 1.000000000000000000, 0.7279177720675241714, 1.000000000000000000),
 ( 1.000000000000000000, 0.7263769756471946115, 1.000000000000000000),
 ( 1.000000000000000000, 0.7234575735669767083, 1.000000000000000000),
 ( 1.000000000000000000, 0.7220742453523991689, 1.000000000000000000),
 ( 1.000000000000000000, 0.7155655556167423992, 1.000000000000000000),
 ( 1.000000000000000000, 0.7116656400988581321, 1.000000000000000000),
 ( 1.000000000000000000, 0.7088249914908492100, 1.000000000000000000),
 ( 1.000000000000000000, 0.7083584775623817942, 1.000000000000000000),
 ( 1.000000000000000000, 0.7076383381209198076, 1.000000000000000000),
 ( 1.000000000000000000, 0.7073855737940044630, 1.000000000000000000),
 ( 1.000000000000000000, 0.7069609716970313151, 1.000000000000000000),
 ( 1.000000000000000000, 0.7071175024107954066, 1.000000000000000000),
 ( 1.000000000000000000, 0.7082797836801750790, 1.000000000000000000),
 ( 1.000000000000000000, 0.7092855318707916856, 1.000000000000000000),
 ( 1.000000000000000000, 0.7121081611133525113, 1.000000000000000000),
 ( 1.000000000000000000, 0.7139297788701386427, 1.000000000000000000),
 ( 1.000000000000000000, 0.7205123102341589592, 1.000000000000000000),
 ( 1.000000000000000000, 0.7262634879477153360, 1.000000000000000000),
 ( 1.000000000000000000, 0.7362377633225355433, 1.000000000000000000),
 ( 1.000000000000000000, 0.7397880641819555292, 1.000000000000000000),
 ( 1.000000000000000000, 0.7453704836958430224, 1.000000000000000000),
 ( 1.000000000000000000, 0.7472719429557758142, 1.000000000000000000),
 ( 1.000000000000000000, 0.7511059034608574825, 1.000000000000000000),
 ( 1.000000000000000000, 0.7530430930858292848, 1.000000000000000000),
 ( 1.000000000000000000, 0.7627925276597339321, 1.000000000000000000),
 ( 1.000000000000000000, 0.7707906794718482058, 1.000000000000000000),
 ( 1.000000000000000000, 0.7824407450661361452, 1.000000000000000000),
 ( 1.000000000000000000, 0.7862798113962640167, 1.000000000000000000),
 ( 1.000000000000000000, 0.7935920352645898790, 1.000000000000000000),
 ( 1.000000000000000000, 0.7970830763616314485, 1.000000000000000000),
 ( 1.000000000000000000, 0.8069453338637414541, 1.000000000000000000),
 ( 1.000000000000000000, 0.8127078027066928501, 1.000000000000000000),
 ( 1.000000000000000000, 0.8173438319342977154, 1.000000000000000000) ) ) 
 REPRESENTATION_ITEM ( '' )  SURFACE ( )  );
#287 = CIRCLE ( 'NONE', #5208, 7.500000000000007105 ) ;
#288 = AXIS2_PLACEMENT_3D ( 'NONE', #7289, #5491, #4381 ) ;
#289 = ORIENTED_EDGE ( 'NONE', *, *, #5265, .F. ) ;
#290 = CARTESIAN_POINT ( 'NONE',  ( -821.1548363108382773, 74.44610204637874062, -143.1996371447159788 ) ) ;
#291 = PLANE ( 'NONE',  #9364 ) ;
#292 = CARTESIAN_POINT ( 'NONE',  ( -13.32222501832919193, 180.2041921146325762, -184.1652315311841051 ) ) ;
#293 = CARTESIAN_POINT ( 'NONE',  ( -1037.392967692951970, 114.2240391150264998, -136.2353035311982126 ) ) ;
#294 = CARTESIAN_POINT ( 'NONE',  ( -372.7969387542311210, 100.6399613739977497, -117.3710749709770198 ) ) ;
#295 = CARTESIAN_POINT ( 'NONE',  ( -7.499999999999979572, -6.999999999999979572, -124.6807709998038405 ) ) ;
#296 = AXIS2_PLACEMENT_3D ( 'NONE', #7544, #3832, #1922 ) ;
#297 = FACE_BOUND ( 'NONE', #8922, .T. ) ;
#298 = ORIENTED_EDGE ( 'NONE', *, *, #7352, .T. ) ;
#299 = CARTESIAN_POINT ( 'NONE',  ( 3.123963502971610252E-13, 164.0000000000000000, -96.42135623730948168 ) ) ;
#300 = CARTESIAN_POINT ( 'NONE',  ( -1060.756016675586807, 112.8516620848305934, -124.6807709998040821 ) ) ;
#301 = CARTESIAN_POINT ( 'NONE',  ( 7.500000000000022204, -9.213203435596451385, -126.4213562373094959 ) ) ;
#302 = CARTESIAN_POINT ( 'NONE',  ( -1037.550865396555764, 105.7975851359348667, -146.0307792196445860 ) ) ;
#303 = DIRECTION ( 'NONE',  ( -1.186840563529527301E-16, 1.000000000000000000, -0.000000000000000000 ) ) ;
#304 = ORIENTED_EDGE ( 'NONE', *, *, #9166, .F. ) ;
#305 = AXIS2_PLACEMENT_3D ( 'NONE', #12094, #1705, #10105 ) ;
#306 = EDGE_LOOP ( 'NONE', ( #4987, #12037, #7872, #11168 ) ) ;
#307 = EDGE_CURVE ( 'NONE', #1954, #154, #9065, .T. ) ;
#308 = FACE_BOUND ( 'NONE', #6793, .T. ) ;
#309 = CARTESIAN_POINT ( 'NONE',  ( -953.8433812051875975, 65.95343150956774991, -149.7857175106634315 ) ) ;
#310 = CARTESIAN_POINT ( 'NONE',  ( -823.8285638327238303, 78.67432280806536937, -89.68077099980398259 ) ) ;
#311 = DIRECTION ( 'NONE',  ( -1.000000000000000000, 0.000000000000000000, 0.000000000000000000 ) ) ;
#312 = DIRECTION ( 'NONE',  ( -1.000000000000000000, 0.000000000000000000, 0.000000000000000000 ) ) ;
#313 = CARTESIAN_POINT ( 'NONE',  ( -854.0803342822151762, 23.97549884981696167, -130.5712005305403238 ) ) ;
#314 = AXIS2_PLACEMENT_3D ( 'NONE', #7746, #6638, #6880 ) ;
#315 = ORIENTED_EDGE ( 'NONE', *, *, #3330, .T. ) ;
#316 = EDGE_LOOP ( 'NONE', ( #9146, #634 ) ) ;
#317 = CARTESIAN_POINT ( 'NONE',  ( -1028.454949082212806, 53.01113643315385104, -113.1262384684094400 ) ) ;
#318 = DIRECTION ( 'NONE',  ( -3.061276722312011504E-17, 1.000000000000000000, 0.000000000000000000 ) ) ;
#319 = CARTESIAN_POINT ( 'NONE',  ( 45.53315400109643463, 12.00000000000000000, -230.3419396193597208 ) ) ;
#320 = CARTESIAN_POINT ( 'NONE',  ( -1038.664246639927342, 43.28664065472985811, -136.2353035311990084 ) ) ;
#321 = EDGE_CURVE ( 'NONE', #10730, #10836, #6230, .T. ) ;
#322 = ORIENTED_EDGE ( 'NONE', *, *, #4849, .T. ) ;
#323 = CYLINDRICAL_SURFACE ( 'NONE', #3336, 7.500000000000007105 ) ;
#324 = CARTESIAN_POINT ( 'NONE',  ( -380.4203626278499542, 64.21146706504150359, -115.5204214313296376 ) ) ;
#325 = ORIENTED_EDGE ( 'NONE', *, *, #5571, .T. ) ;
#326 = CARTESIAN_POINT ( 'NONE',  ( -824.4849247483655290, 73.70682285379986354, -154.6506428397234743 ) ) ;
#327 = ORIENTED_EDGE ( 'NONE', *, *, #355, .T. ) ;
#328 = EDGE_LOOP ( 'NONE', ( #135, #8709, #7075, #7838 ) ) ;
#329 = CARTESIAN_POINT ( 'NONE',  ( -1065.000000000003865, 52.00000000000021316, -126.6442663926290493 ) ) ;
#330 = DIRECTION ( 'NONE',  ( -1.000000000000000000, 0.000000000000000000, 0.000000000000000000 ) ) ;
#331 = DIRECTION ( 'NONE',  ( 1.000000000000000000, 0.000000000000000000, 1.224646799147353207E-16 ) ) ;
#332 = AXIS2_PLACEMENT_3D ( 'NONE', #843, #8325, #8259 ) ;
#333 = DIRECTION ( 'NONE',  ( 0.000000000000000000, -1.156482317317870246E-16, 1.000000000000000000 ) ) ;
#334 = CIRCLE ( 'NONE', #5074, 57.99999999999999289 ) ;
#335 = CARTESIAN_POINT ( 'NONE',  ( -1061.468168685228193, 92.73456844357777129, -96.78565065507918064 ) ) ;
#336 = LINE ( 'NONE', #1445, #8050 ) ;
#337 = CARTESIAN_POINT ( 'NONE',  ( 19.00000000000000000, 197.0000000000000000, -124.6807709998038405 ) ) ;
#338 = VERTEX_POINT ( 'NONE', #2508 ) ;
#339 = LINE ( 'NONE', #9047, #1075 ) ;
#340 = EDGE_CURVE ( 'NONE', #2669, #5042, #5605, .T. ) ;
#341 = CIRCLE ( 'NONE', #6268, 30.00000000000021316 ) ;
#342 = EDGE_CURVE ( 'NONE', #12110, #8166, #11773, .T. ) ;
#343 =( NAMED_UNIT ( * ) PLANE_ANGLE_UNIT ( ) SI_UNIT ( $, .RADIAN. ) );
#344 = EDGE_LOOP ( 'NONE', ( #2553, #10547, #8461, #7126 ) ) ;
#345 = CARTESIAN_POINT ( 'NONE',  ( -1055.782959745578182, 85.17781532426863578, -95.06748246948041015 ) ) ;
#346 = EDGE_LOOP ( 'NONE', ( #11443, #5040 ) ) ;
#347 = CARTESIAN_POINT ( 'NONE',  ( -1021.743962174751232, 119.2557508373789403, -124.6807709998040110 ) ) ;
#348 = CARTESIAN_POINT ( 'NONE',  ( 154.5043356068769071, 12.00000000000000000, -109.5666613060171670 ) ) ;
#349 = EDGE_CURVE ( 'NONE', #7831, #3787, #3152, .T. ) ;
#350 = CARTESIAN_POINT ( 'NONE',  ( 151.3258811035896656, 12.00000000000000000, -48.63263083939796871 ) ) ;
#351 = AXIS2_PLACEMENT_3D ( 'NONE', #10311, #1910, #9449 ) ;
#352 = DIRECTION ( 'NONE',  ( 0.000000000000000000, 0.000000000000000000, 1.000000000000000000 ) ) ;
#353 = DIRECTION ( 'NONE',  ( -0.000000000000000000, -1.000000000000000000, 0.000000000000000000 ) ) ;
#354 = CARTESIAN_POINT ( 'NONE',  ( -1048.438004920983303, 39.66697241395321782, -124.6807709998044800 ) ) ;
#355 = EDGE_CURVE ( 'NONE', #1262, #3617, #2145, .T. ) ;
#356 = DIRECTION ( 'NONE',  ( 0.000000000000000000, -1.000000000000000000, -7.930164461608263644E-17 ) ) ;
#357 = CIRCLE ( 'NONE', #7273, 7.499999999999992895 ) ;
#358 = ORIENTED_EDGE ( 'NONE', *, *, #9645, .T. ) ;
#359 = FACE_OUTER_BOUND ( 'NONE', #1203, .T. ) ;
#360 = PLANE ( 'NONE',  #530 ) ;
#361 = CARTESIAN_POINT ( 'NONE',  ( -1024.691966601151762, 118.8493250655917564, -126.6442663926291061 ) ) ;
#362 = AXIS2_PLACEMENT_3D ( 'NONE', #5126, #8886, #3258 ) ;
#363 = CARTESIAN_POINT ( 'NONE',  ( -375.0000000000000000, 81.99999999999995737, -89.68077099980384048 ) ) ;
#364 = CARTESIAN_POINT ( 'NONE',  ( -374.9435208796285224, 79.09557628031252818, -94.85325544560421918 ) ) ;
#365 = ORIENTED_EDGE ( 'NONE', *, *, #10686, .T. ) ;
#366 = APPLICATION_CONTEXT ( 'automotive_design' ) ;
#367 = CIRCLE ( 'NONE', #4729, 7.500000000000007105 ) ;
#368 = VERTEX_POINT ( 'NONE', #31 ) ;
#369 = CARTESIAN_POINT ( 'NONE',  ( -90.00000000000000000, 152.0000000000000000, -126.4213562373088564 ) ) ;
#370 = FACE_BOUND ( 'NONE', #3925, .T. ) ;
#371 = CIRCLE ( 'NONE', #8725, 7.500000000000007105 ) ;
#372 = DIRECTION ( 'NONE',  ( 0.000000000000000000, -1.000000000000000000, -1.850371707708592551E-14 ) ) ;
#373 = CARTESIAN_POINT ( 'NONE',  ( -22.49999999999997868, -9.213203435596451385, -126.4213562373092685 ) ) ;
#374 = CARTESIAN_POINT ( 'NONE',  ( -827.5978224575839022, 75.37295367873073815, -94.68020981275554959 ) ) ;
#375 =( NAMED_UNIT ( * ) SI_UNIT ( $, .STERADIAN. ) SOLID_ANGLE_UNIT ( ) );
#376 = CIRCLE ( 'NONE', #5908, 7.500000000000012434 ) ;
#377 = EDGE_LOOP ( 'NONE', ( #4540, #1681, #1210, #5686, #11186, #2942, #6085, #5745, #3833, #8762 ) ) ;
#378 = CARTESIAN_POINT ( 'NONE',  ( -1062.923339974281134, 49.86928741160674150, -136.2353035311989515 ) ) ;
#379 = ORIENTED_EDGE ( 'NONE', *, *, #11461, .F. ) ;
#380 = ORIENTED_EDGE ( 'NONE', *, *, #161, .F. ) ;
#381 = DIRECTION ( 'NONE',  ( -0.000000000000000000, 1.000000000000000000, -0.000000000000000000 ) ) ;
#382 = CARTESIAN_POINT ( 'NONE',  ( -1017.158871447982051, 53.64146012065780411, -122.7172756069791717 ) ) ;
#383 = EDGE_LOOP ( 'NONE', ( #2203, #8907 ) ) ;
#384 = CARTESIAN_POINT ( 'NONE',  ( -151.3258811035894098, 12.00000000000000000, -48.63263083939678921 ) ) ;
#385 = CARTESIAN_POINT ( 'NONE',  ( -822.5313098515729280, 73.83434793536794416, -154.6477719089843390 ) ) ;
#386 = ORIENTED_EDGE ( 'NONE', *, *, #9875, .T. ) ;
#387 = ORIENTED_EDGE ( 'NONE', *, *, #9652, .F. ) ;
#388 = CARTESIAN_POINT ( 'NONE',  ( -976.2517683711888594, 35.25052392388814582, -122.7172756069790296 ) ) ;
#389 = EDGE_CURVE ( 'NONE', #4400, #11584, #1104, .T. ) ;
#390 = DIRECTION ( 'NONE',  ( 0.000000000000000000, 0.000000000000000000, -1.000000000000000000 ) ) ;
#391 = EDGE_CURVE ( 'NONE', #7319, #11283, #7095, .T. ) ;
#392 = CARTESIAN_POINT ( 'NONE',  ( 0.07661102881317549684, 6.914460432017338398, 6.023803224821312696 ) ) ;
#393 = CARTESIAN_POINT ( 'NONE',  ( -1025.928429817214464, 97.79385104913474436, -96.78565065507955012 ) ) ;
#394 = CYLINDRICAL_SURFACE ( 'NONE', #10869, 134.9999999999999716 ) ;
#395 = ORIENTED_EDGE ( 'NONE', *, *, #7971, .T. ) ;
#396 = ORIENTED_EDGE ( 'NONE', *, *, #11359, .T. ) ;
#397 = CARTESIAN_POINT ( 'NONE',  ( -795.0000000000002274, 98.77454568802498613, -99.57582448894500260 ) ) ;
#398 = CARTESIAN_POINT ( 'NONE',  ( -380.0318359341034693, 100.5075656702939142, -132.3766003259852084 ) ) ;
#399 = CARTESIAN_POINT ( 'NONE',  ( -951.4198147059589701, 125.0824040815807194, -124.6807709998040252 ) ) ;
#400 = CYLINDRICAL_SURFACE ( 'NONE', #7484, 7.500000000000007105 ) ;
#401 = EDGE_CURVE ( 'NONE', #10520, #8134, #578, .T. ) ;
#402 = CARTESIAN_POINT ( 'NONE',  ( -180.0000000000000000, 12.00000000000001421, -126.4213562373082453 ) ) ;
#403 = EDGE_CURVE ( 'NONE', #4980, #6173, #8091, .T. ) ;
#404 = FACE_BOUND ( 'NONE', #5340, .T. ) ;
#405 = CARTESIAN_POINT ( 'NONE',  ( 126.4213562373094959, -6.000000000000000000, -6.938893903907228378E-15 ) ) ;
#406 = PRODUCT_DEFINITION ( 'UNKNOWN', '', #11578, #8636 ) ;
#407 = FACE_OUTER_BOUND ( 'NONE', #12097, .T. ) ;
#408 = ORIENTED_EDGE ( 'NONE', *, *, #9663, .F. ) ;
#409 = CARTESIAN_POINT ( 'NONE',  ( 1.874378101782966050E-12, 152.0000000000000000, 53.57864376269051832 ) ) ;
#410 = CARTESIAN_POINT ( 'NONE',  ( -1017.810720698608179, 119.7719591276206046, -126.6442663926290493 ) ) ;
#411 = DIRECTION ( 'NONE',  ( -0.000000000000000000, -1.000000000000000000, -0.000000000000000000 ) ) ;
#412 = AXIS2_PLACEMENT_3D ( 'NONE', #9186, #721, #4497 ) ;
#413 = CARTESIAN_POINT ( 'NONE',  ( 1.387778780781445676E-14, -494.9999999999998863, 126.4213562373094959 ) ) ;
#414 = EDGE_CURVE ( 'NONE', #957, #11231, #4747, .T. ) ;
#415 = ORIENTED_EDGE ( 'NONE', *, *, #2463, .T. ) ;
#416 = CARTESIAN_POINT ( 'NONE',  ( 19.96510381999703654, 179.6655525025668680, -123.2864411696423019 ) ) ;
#417 = DIRECTION ( 'NONE',  ( 2.081668171172161734E-17, 4.930380657631307143E-31, -1.000000000000000000 ) ) ;
#418 = AXIS2_PLACEMENT_3D ( 'NONE', #4659, #2540, #5635 ) ;
#419 = CARTESIAN_POINT ( 'NONE',  ( -373.3204616456844747, 97.25197993938448349, -149.1095482086399784 ) ) ;
#420 = DIRECTION ( 'NONE',  ( -0.000000000000000000, 1.000000000000000000, 0.000000000000000000 ) ) ;
#421 = DIRECTION ( 'NONE',  ( 0.000000000000000000, -1.189524669241239115E-16, 1.000000000000000000 ) ) ;
#422 = LINE ( 'NONE', #11515, #6475 ) ;
#423 = AXIS2_PLACEMENT_3D ( 'NONE', #2783, #4705, #7030 ) ;
#424 = EDGE_LOOP ( 'NONE', ( #6274, #101, #7246, #3774 ) ) ;
#425 = CARTESIAN_POINT ( 'NONE',  ( -901.9718911164696920, 59.00785292138922244, -136.2353035311984115 ) ) ;
#426 = APPLICATION_CONTEXT ( 'automotive_design' ) ;
#427 = VECTOR ( 'NONE', #2802, 999.9999999999998863 ) ;
#428 = ORIENTED_EDGE ( 'NONE', *, *, #8066, .T. ) ;
#429 = CARTESIAN_POINT ( 'NONE',  ( 30.00000000000000000, -492.9999999999998863, -30.00000000000000000 ) ) ;
#430 = CARTESIAN_POINT ( 'NONE',  ( -1062.996098538733122, 47.98024286075321498, -118.7903414690683377 ) ) ;
#431 = DIRECTION ( 'NONE',  ( 0.000000000000000000, 0.000000000000000000, 1.000000000000000000 ) ) ;
#432 = CARTESIAN_POINT ( 'NONE',  ( -824.1522960622456822, 83.67452213711085562, -95.25851046848316628 ) ) ;
#433 = CARTESIAN_POINT ( 'NONE',  ( -818.8285638327243987, 78.67432280806558254, -94.73795703228648790 ) ) ;
#434 = EDGE_LOOP ( 'NONE', ( #6079, #8343 ) ) ;
#435 = ORIENTED_EDGE ( 'NONE', *, *, #33, .T. ) ;
#436 = FACE_OUTER_BOUND ( 'NONE', #2758, .T. ) ;
#437 = CARTESIAN_POINT ( 'NONE',  ( -1021.637154595298057, 53.81063926482157456, -126.6442663926291630 ) ) ;
#438 = CARTESIAN_POINT ( 'NONE',  ( 0.000000000000000000, 1.502314598737159426E-15, -9.000000000000000000 ) ) ;
#439 = CARTESIAN_POINT ( 'NONE',  ( -818.8285638327238303, 78.67432280806571043, -144.4023295390032899 ) ) ;
#440 = CIRCLE ( 'NONE', #6189, 4.000000000000003553 ) ;
#441 = CARTESIAN_POINT ( 'NONE',  ( -8.500000000000003553, 24.00000000000002132, -126.4213562373094959 ) ) ;
#442 = CARTESIAN_POINT ( 'NONE',  ( -90.00000000000000000, 139.9999999999999716, -126.4213562373088564 ) ) ;
#443 = CARTESIAN_POINT ( 'NONE',  ( -1031.329434936836833, 101.6864263019767378, -99.57582448894520155 ) ) ;
#444 = CARTESIAN_POINT ( 'NONE',  ( -35.00000000000000000, 12.00000000000000000, 81.78351099501843180 ) ) ;
#445 = DIRECTION ( 'NONE',  ( 0.000000000000000000, 0.000000000000000000, -1.000000000000000000 ) ) ;
#446 = ADVANCED_FACE ( 'NONE', ( #2952 ), #990, .T. ) ;
#447 = ORIENTED_EDGE ( 'NONE', *, *, #3448, .T. ) ;
#448 = DIRECTION ( 'NONE',  ( -1.000000000000000000, 0.000000000000000000, 0.000000000000000000 ) ) ;
#449 = AXIS2_PLACEMENT_3D ( 'NONE', #6036, #2435, #448 ) ;
#450 = DIRECTION ( 'NONE',  ( 0.000000000000000000, 0.000000000000000000, 1.000000000000000000 ) ) ;
#451 = CIRCLE ( 'NONE', #3416, 7.500000000000007105 ) ;
#452 = ORIENTED_EDGE ( 'NONE', *, *, #4862, .T. ) ;
#453 = CARTESIAN_POINT ( 'NONE',  ( -828.7969121913764639, 79.32510138126919230, -154.5423082524717699 ) ) ;
#454 = CARTESIAN_POINT ( 'NONE',  ( -1038.158164256576356, 71.32123499372119113, -95.06748246948035330 ) ) ;
#455 = DIRECTION ( 'NONE',  ( 0.000000000000000000, -1.000000000000000000, -7.930164461608263644E-17 ) ) ;
#456 = CARTESIAN_POINT ( 'NONE',  ( -823.7180591916866206, 117.1502831467254993, -130.5712005305406080 ) ) ;
#457 = CARTESIAN_POINT ( 'NONE',  ( -20.81528965651789420, 181.2703058956580264, -123.7202784472551258 ) ) ;
#458 = DIRECTION ( 'NONE',  ( -0.000000000000000000, -1.000000000000000000, -0.000000000000000000 ) ) ;
#459 = CARTESIAN_POINT ( 'NONE',  ( 19.83353877203827764, 180.5116607636902302, -127.2558091114354966 ) ) ;
#460 = CARTESIAN_POINT ( 'NONE',  ( 19.88442870626286307, 179.4513098237186455, -122.5333155736647655 ) ) ;
#461 = AXIS2_PLACEMENT_3D ( 'NONE', #12105, #7277, #8143 ) ;
#462 = VECTOR ( 'NONE', #11784, 1000.000000000000000 ) ;
#463 = AXIS2_PLACEMENT_3D ( 'NONE', #244, #1196, #4029 ) ;
#464 = CARTESIAN_POINT ( 'NONE',  ( -795.0000000000020464, 111.6133447792289530, -118.7903414690682524 ) ) ;
#465 = CARTESIAN_POINT ( 'NONE',  ( 20.00000000000000000, 197.0000000000000000, -124.6807709998038405 ) ) ;
#466 = CARTESIAN_POINT ( 'NONE',  ( -824.1545993022709808, 83.67440335600066703, -104.7509849144497736 ) ) ;
#467 = CARTESIAN_POINT ( 'NONE',  ( -795.0000000000048885, 52.00000000000024158, -124.6807709998040821 ) ) ;
#468 = EDGE_CURVE ( 'NONE', #6717, #8440, #6310, .T. ) ;
#469 = LINE ( 'NONE', #4263, #6510 ) ;
#470 = CARTESIAN_POINT ( 'NONE',  ( 7.500000000000000000, 5.196152422706624918, 8.999999999999998224 ) ) ;
#471 = ORIENTED_EDGE ( 'NONE', *, *, #4119, .T. ) ;
#472 = DIRECTION ( 'NONE',  ( -1.000000000000000000, -0.000000000000000000, -0.000000000000000000 ) ) ;
#473 = CARTESIAN_POINT ( 'NONE',  ( 1.387778780781445676E-14, 163.9999999999999716, 126.4213562373094959 ) ) ;
#474 = CIRCLE ( 'NONE', #2458, 7.500000000000007105 ) ;
#475 = VECTOR ( 'NONE', #10063, 1000.000000000000000 ) ;
#476 = DIRECTION ( 'NONE',  ( 0.000000000000000000, 1.632680918566399772E-14, -1.000000000000000000 ) ) ;
#477 = CARTESIAN_POINT ( 'NONE',  ( -955.0000000000038654, 102.0000000000005400, -124.6807709998041531 ) ) ;
#478 = ADVANCED_FACE ( 'NONE', ( #7705, #4803, #8575, #5910, #10363, #9558, #10543, #5725, #8699, #6657, #2827 ), #11414, .F. ) ;
#479 = DIRECTION ( 'NONE',  ( 1.000000000000000000, 1.486905836551548832E-16, -0.000000000000000000 ) ) ;
#480 = EDGE_LOOP ( 'NONE', ( #1423, #3316 ) ) ;
#481 = VERTEX_POINT ( 'NONE', #1901 ) ;
#482 = VECTOR ( 'NONE', #7675, 1000.000000000000000 ) ;
#483 = CIRCLE ( 'NONE', #3067, 7.500000000000007105 ) ;
#484 = FACE_BOUND ( 'NONE', #2793, .T. ) ;
#485 = CARTESIAN_POINT ( 'NONE',  ( -902.6139906877482417, 77.75433758651681160, -152.5758913445294809 ) ) ;
#486 = CARTESIAN_POINT ( 'NONE',  ( -818.9962482452939412, 77.37998253221861944, -144.1405054422210981 ) ) ;
#487 = ORIENTED_EDGE ( 'NONE', *, *, #11842, .T. ) ;
#488 = CARTESIAN_POINT ( 'NONE',  ( -374.5655304648819879, 89.79463081985890938, -153.3305951811361751 ) ) ;
#489 = CARTESIAN_POINT ( 'NONE',  ( 0.5595136366802130334, -4.349754824395698272, 9.000000000000000000 ) ) ;
#490 = ADVANCED_FACE ( 'NONE', ( #99 ), #10651, .T. ) ;
#492 = ADVANCED_FACE ( 'NONE', ( #8638 ), #1164, .F. ) ;
#491 = CARTESIAN_POINT ( 'NONE',  ( -20.90635653397698590, 181.5182364730088125, -122.6997973820476489 ) ) ;
#493 = EDGE_LOOP ( 'NONE', ( #7203, #9839, #8059, #6199 ) ) ;
#494 = CARTESIAN_POINT ( 'NONE',  ( -1013.844210246968942, 57.79547239392000790, -141.4553492942758908 ) ) ;
#495 = VERTEX_POINT ( 'NONE', #7765 ) ;
#496 = EDGE_CURVE ( 'NONE', #546, #9681, #11781, .T. ) ;
#497 = CARTESIAN_POINT ( 'NONE',  ( -19.97664783916611952, 180.3484222408143296, -126.1556734819005925 ) ) ;
#498 = ORIENTED_EDGE ( 'NONE', *, *, #8039, .T. ) ;
#499 = CARTESIAN_POINT ( 'NONE',  ( -827.5988398165042099, 81.97491382366440860, -95.05718603569194158 ) ) ;
#500 =( GEOMETRIC_REPRESENTATION_CONTEXT ( 3 ) GLOBAL_UNCERTAINTY_ASSIGNED_CONTEXT ( ( #6769 ) ) GLOBAL_UNIT_ASSIGNED_CONTEXT ( ( #4246, #9639, #11099 ) ) REPRESENTATION_CONTEXT ( 'NONE', 'WORKASPACE' ) );
#501 = CARTESIAN_POINT ( 'NONE',  ( -379.1619848709567577, 102.0000000000000284, -123.4679443962072725 ) ) ;
#502 = VERTEX_POINT ( 'NONE', #6093 ) ;
#503 = AXIS2_PLACEMENT_3D ( 'NONE', #6514, #3590, #1821 ) ;
#504 = EDGE_CURVE ( 'NONE', #9388, #1374, #2263, .T. ) ;
#505 = VERTEX_POINT ( 'NONE', #2202 ) ;
#506 = CARTESIAN_POINT ( 'NONE',  ( -998.0431609429218724, 37.14019503514174403, -126.6442663926292340 ) ) ;
#507 = CARTESIAN_POINT ( 'NONE',  ( -27.99999999999999645, -6.000000000000000000, 27.99999999999999645 ) ) ;
#508 = LINE ( 'NONE', #9976, #3240 ) ;
#509 = PRODUCT_DEFINITION_FORMATION_WITH_SPECIFIED_SOURCE ( 'ANY', '', #2792, .NOT_KNOWN. ) ;
#510 = PLANE ( 'NONE',  #8625 ) ;
#511 = VECTOR ( 'NONE', #1443, 1000.000000000000000 ) ;
#512 = CARTESIAN_POINT ( 'NONE',  ( -974.6181169426257611, 104.3135445892214506, -99.57582448894483207 ) ) ;
#513 = CARTESIAN_POINT ( 'NONE',  ( -19.99999999999999645, 177.7115707886035807, -124.6807709997916334 ) ) ;
#514 = CARTESIAN_POINT ( 'NONE',  ( -374.8923245633905026, 85.92087493068839876, -95.01038614168759011 ) ) ;
#515 = ORIENTED_EDGE ( 'NONE', *, *, #1701, .T. ) ;
#516 = DIRECTION ( 'NONE',  ( 1.000000000000000000, 0.000000000000000000, 0.000000000000000000 ) ) ;
#517 = CARTESIAN_POINT ( 'NONE',  ( -374.9998907128388623, 83.71581840400844499, -94.68015511488202662 ) ) ;
#518 = ORIENTED_EDGE ( 'NONE', *, *, #8104, .T. ) ;
#519 = DIRECTION ( 'NONE',  ( -0.000000000000000000, 1.000000000000000000, 7.930164461608263644E-17 ) ) ;
#520 = CARTESIAN_POINT ( 'NONE',  ( 7.750278301654327992E-16, 197.0000000000000000, -124.6807709998038405 ) ) ;
#521 = ORIENTED_EDGE ( 'NONE', *, *, #11514, .T. ) ;
#522 = DIRECTION ( 'NONE',  ( 0.000000000000000000, 0.000000000000000000, 1.000000000000000000 ) ) ;
#523 = CARTESIAN_POINT ( 'NONE',  ( -903.0443340174317655, 90.92133391050421665, -94.48732055948569553 ) ) ;
#524 = TOROIDAL_SURFACE ( 'NONE', #1147, 44.00000000000000711, 1.000000000000000000 ) ;
#525 = CARTESIAN_POINT ( 'NONE',  ( 9.381075359908434252E-13, 152.0000000000000000, -43.92135623730948879 ) ) ;
#526 = CARTESIAN_POINT ( 'NONE',  ( -1017.810720698608179, 119.7719591276206046, -126.6442663926290493 ) ) ;
#527 = CARTESIAN_POINT ( 'NONE',  ( 19.83120603885254951, 180.1820437873792287, -127.2737130629590041 ) ) ;
#528 = DIRECTION ( 'NONE',  ( -8.163404592832031500E-17, 1.000000000000000000, 0.000000000000000000 ) ) ;
#529 = CARTESIAN_POINT ( 'NONE',  ( -119.9999999999999858, 24.00000000000001421, -126.4213562373086575 ) ) ;
#530 = AXIS2_PLACEMENT_3D ( 'NONE', #4144, #3201, #7285 ) ;
#531 = CARTESIAN_POINT ( 'NONE',  ( -819.1462522098552199, 76.91297450996658824, -144.0236343770278609 ) ) ;
#532 = VECTOR ( 'NONE', #8116, 1000.000000000000000 ) ;
#533 = FACE_BOUND ( 'NONE', #4273, .T. ) ;
#534 = DIRECTION ( 'NONE',  ( 0.000000000000000000, 1.000000000000000000, 0.000000000000000000 ) ) ;
#535 = CARTESIAN_POINT ( 'NONE',  ( -823.4987033863208126, 83.67412160126858112, -95.25369430085760314 ) ) ;
#536 = ORIENTED_EDGE ( 'NONE', *, *, #1166, .F. ) ;
#537 = FACE_OUTER_BOUND ( 'NONE', #8170, .T. ) ;
#538 = CARTESIAN_POINT ( 'NONE',  ( -904.2101318206010774, 125.2895275102983419, -122.7172756069790580 ) ) ;
#539 = FACE_OUTER_BOUND ( 'NONE', #6413, .T. ) ;
#540 = DIRECTION ( 'NONE',  ( 0.000000000000000000, -1.000000000000000000, -7.930164461608263644E-17 ) ) ;
#541 = CARTESIAN_POINT ( 'NONE',  ( 4.808665244885994618E-14, -494.9999999999998863, 141.4213562373094817 ) ) ;
#542 = EDGE_CURVE ( 'NONE', #9452, #8983, #6330, .T. ) ;
#543 = CARTESIAN_POINT ( 'NONE',  ( 3.133148353965215262E-13, 164.0000000000000000, -103.9213562373094817 ) ) ;
#544 = EDGE_CURVE ( 'NONE', #10381, #12119, #6034, .T. ) ;
#545 = ORIENTED_EDGE ( 'NONE', *, *, #11311, .F. ) ;
#546 = VERTEX_POINT ( 'NONE', #9798 ) ;
#547 = CARTESIAN_POINT ( 'NONE',  ( 19.96803729195536548, 180.8767316306619932, -123.3312649246138051 ) ) ;
#548 = AXIS2_PLACEMENT_3D ( 'NONE', #8993, #5805, #1125 ) ;
#549 = DIRECTION ( 'NONE',  ( -1.000000000000000000, -3.061276722312011504E-17, 0.000000000000000000 ) ) ;
#550 = DIRECTION ( 'NONE',  ( 0.000000000000000000, -1.000000000000000000, -7.930164461608263644E-17 ) ) ;
#551 = CARTESIAN_POINT ( 'NONE',  ( -370.0721644750066730, 107.8006199747635492, -130.5475387910841221 ) ) ;
#552 = CIRCLE ( 'NONE', #6873, 0.9999999999999986677 ) ;
#553 = ADVANCED_FACE ( 'NONE', ( #5206 ), #2432, .T. ) ;
#554 = CARTESIAN_POINT ( 'NONE',  ( 151.3258811035896656, 12.00000000000000000, -48.63263083939796871 ) ) ;
#555 = DIRECTION ( 'NONE',  ( -8.163404592832030268E-17, 1.000000000000000000, -0.000000000000000000 ) ) ;
#556 = CARTESIAN_POINT ( 'NONE',  ( 19.03136272649511085, 180.2041921146316668, -134.6807709998038547 ) ) ;
#557 = CARTESIAN_POINT ( 'NONE',  ( -824.4876953351460998, 73.70726043279957196, -94.71087641695557124 ) ) ;
#558 = SURFACE_STYLE_USAGE ( .BOTH. , #4395 ) ;
#559 = VERTEX_POINT ( 'NONE', #337 ) ;
#560 = LINE ( 'NONE', #4380, #7867 ) ;
#561 = CARTESIAN_POINT ( 'NONE',  ( -927.9936929689694125, 74.21188826700395680, -149.7857175106638863 ) ) ;
#562 = VECTOR ( 'NONE', #6726, 1000.000000000000000 ) ;
#563 = ORIENTED_EDGE ( 'NONE', *, *, #496, .T. ) ;
#564 = EDGE_CURVE ( 'NONE', #918, #10860, #2578, .T. ) ;
#565 = FACE_OUTER_BOUND ( 'NONE', #10182, .T. ) ;
#566 = EDGE_CURVE ( 'NONE', #8781, #8293, #8892, .T. ) ;
#567 = CARTESIAN_POINT ( 'NONE',  ( -19.85757705203717549, 179.1763491573645979, -127.0639759997010714 ) ) ;
#568 = AXIS2_PLACEMENT_3D ( 'NONE', #5738, #2909, #4137 ) ;
#569 = VERTEX_POINT ( 'NONE', #9980 ) ;
#570 = CARTESIAN_POINT ( 'NONE',  ( -828.7958589970872936, 79.33211491968606310, -94.81972313272032693 ) ) ;
#571 = AXIS2_PLACEMENT_3D ( 'NONE', #8163, #1546, #11066 ) ;
#572 = DIRECTION ( 'NONE',  ( 0.000000000000000000, 0.000000000000000000, 1.000000000000000000 ) ) ;
#573 = ORIENTED_EDGE ( 'NONE', *, *, #3270, .F. ) ;
#574 = B_SPLINE_CURVE_WITH_KNOTS ( 'NONE', 3,
 ( #6859, #1412, #10623, #7851, #11679, #11625, #6974, #2280, #11742, #8936, #3144, #10680, #1355, #2218 ),
 .UNSPECIFIED., .F., .F.,
 ( 4, 2, 2, 2, 2, 2, 4 ),
 ( 0.005787645201702338975, 0.006295307287268509314, 0.006802969372834680520, 0.007818293543967111403, 0.008833617715099544021, 0.009341279800665706554, 0.009848941886231869086 ),
 .UNSPECIFIED. ) ;
#575 = CARTESIAN_POINT ( 'NONE',  ( -955.0000000000038654, 82.00000000000036948, -124.6807709998041673 ) ) ;
#576 = ORIENTED_EDGE ( 'NONE', *, *, #988, .T. ) ;
#577 = CARTESIAN_POINT ( 'NONE',  ( 4.808665244885994618E-14, -492.9999999999998863, 141.4213562373094817 ) ) ;
#578 = CIRCLE ( 'NONE', #1190, 7.500000000000007105 ) ;
#579 = DIRECTION ( 'NONE',  ( -2.081668171172161734E-17, -4.930380657631307143E-31, 1.000000000000000000 ) ) ;
#580 = EDGE_CURVE ( 'NONE', #6384, #8630, #3180, .T. ) ;
#581 = CARTESIAN_POINT ( 'NONE',  ( -994.8066578865433485, 80.00401887192406036, -94.48732055948607922 ) ) ;
#582 = DIRECTION ( 'NONE',  ( 1.776356839400250465E-15, 0.000000000000000000, 1.000000000000000000 ) ) ;
#583 = CARTESIAN_POINT ( 'NONE',  ( -7.500000000000004441, 197.0000000000000000, -124.6807709998038405 ) ) ;
#584 = CARTESIAN_POINT ( 'NONE',  ( -35.00000000000000000, 2.012279232133096230E-14, -124.6807709998040110 ) ) ;
#585 = DIRECTION ( 'NONE',  ( -1.186840563529527301E-16, 1.000000000000000000, -0.000000000000000000 ) ) ;
#586 = VERTEX_POINT ( 'NONE', #7135 ) ;
#587 = CARTESIAN_POINT ( 'NONE',  ( -21.05657978152897769, 178.8587358379057548, -125.5860039436037567 ) ) ;
#588 =( NAMED_UNIT ( * ) SI_UNIT ( $, .STERADIAN. ) SOLID_ANGLE_UNIT ( ) );
#589 = DIRECTION ( 'NONE',  ( 1.000000000000000000, 2.040851148208007875E-17, 0.000000000000000000 ) ) ;
#590 = CARTESIAN_POINT ( 'NONE',  ( -89.99999999999998579, -9.213203435596451385, -126.4213562373088564 ) ) ;
#591 = ORIENTED_EDGE ( 'NONE', *, *, #3649, .T. ) ;
#592 = CARTESIAN_POINT ( 'NONE',  ( -826.3386627754631490, 83.01093823284401196, -154.1821612695491979 ) ) ;
#593 = CARTESIAN_POINT ( 'NONE',  ( -902.6139906877451722, 77.75433758651645633, -96.78565065507919485 ) ) ;
#594 = DIRECTION ( 'NONE',  ( -0.000000000000000000, 1.000000000000000000, -0.000000000000000000 ) ) ;
#595 = PLANE ( 'NONE',  #12120 ) ;
#596 = FACE_OUTER_BOUND ( 'NONE', #11058, .T. ) ;
#597 = CARTESIAN_POINT ( 'NONE',  ( -828.7636281597782499, 77.85463023298294161, -144.2471423470011018 ) ) ;
#598 = B_SPLINE_CURVE_WITH_KNOTS ( 'NONE', 3,
 ( #6314, #1680, #9286, #7245, #826, #4597, #888, #8437, #5439, #11267, #7428, #8371, #4716, #2601, #5375, #11011, #757, #9151, #3650, #4535 ),
 .UNSPECIFIED., .F., .F.,
 ( 4, 2, 2, 2, 2, 2, 2, 2, 2, 4 ),
 ( 0.009933187713138447172, 0.01060625352217340472, 0.01094278642669084187, 0.01127931933120827901, 0.01195238514024315329, 0.01262545094927802758, 0.01329851675831290360, 0.01397158256734777788, 0.01464464837638265217, 0.01531771418541752645 ),
 .UNSPECIFIED. ) ;
#599 = CARTESIAN_POINT ( 'NONE',  ( 1.561981751485805177E-12, 163.9999999999999716, 23.57864376269051832 ) ) ;
#600 = CARTESIAN_POINT ( 'NONE',  ( -817.1493800258449482, 27.50875274330016751, -124.6807709998041815 ) ) ;
#601 = EDGE_LOOP ( 'NONE', ( #8052, #9724 ) ) ;
#602 = FACE_OUTER_BOUND ( 'NONE', #11018, .T. ) ;
#603 = CARTESIAN_POINT ( 'NONE',  ( -1037.337636019038655, 116.9882293220588991, -122.7172756069792001 ) ) ;
#604 = DIRECTION ( 'NONE',  ( 0.000000000000000000, 0.000000000000000000, 1.000000000000000000 ) ) ;
#605 = CARTESIAN_POINT ( 'NONE',  ( 1.562900236585165577E-12, 152.0000000000000000, 16.07864376269051121 ) ) ;
#606 = FACE_OUTER_BOUND ( 'NONE', #11571, .T. ) ;
#607 = B_SPLINE_CURVE_WITH_KNOTS ( 'NONE', 3,
 ( #7578, #11349, #8864, #209, #10602, #5906, #1215, #438 ),
 .UNSPECIFIED., .F., .F.,
 ( 4, 2, 2, 4 ),
 ( 0.02518894968643274959, 0.02782118486451494455, 0.02913730245355604029, 0.03045342004259713950 ),
 .UNSPECIFIED. ) ;
#608 = CARTESIAN_POINT ( 'NONE',  ( 20.00048861043547177, 181.7193014332009113, -124.6844417253709025 ) ) ;
#609 = VERTEX_POINT ( 'NONE', #9044 ) ;
#610 = CARTESIAN_POINT ( 'NONE',  ( 19.89275938512204078, 181.1945314693525972, -122.6057198881955941 ) ) ;
#611 = AXIS2_PLACEMENT_3D ( 'NONE', #3672, #6457, #11093 ) ;
#612 = CARTESIAN_POINT ( 'NONE',  ( -19.97551221440360436, 178.0138700112367758, -123.6762749394707441 ) ) ;
#613 = FACE_BOUND ( 'NONE', #10660, .T. ) ;
#614 = CARTESIAN_POINT ( 'NONE',  ( -1020.082665824768128, 80.34198733739798115, -154.2940595301280950 ) ) ;
#615 = DIRECTION ( 'NONE',  ( 0.000000000000000000, 0.000000000000000000, -1.000000000000000000 ) ) ;
#616 = EDGE_CURVE ( 'NONE', #4019, #1329, #9737, .T. ) ;
#617 = DIRECTION ( 'NONE',  ( 0.000000000000000000, 1.000000000000000000, 0.000000000000000000 ) ) ;
#618 = DIRECTION ( 'NONE',  ( -0.000000000000000000, -1.000000000000000000, -1.757987137413040192E-14 ) ) ;
#619 = ORIENTED_EDGE ( 'NONE', *, *, #2215, .T. ) ;
#620 = DIRECTION ( 'NONE',  ( -8.163404592832030268E-17, 1.000000000000000000, -0.000000000000000000 ) ) ;
#621 = CIRCLE ( 'NONE', #9099, 7.500000000000007105 ) ;
#622 = ADVANCED_FACE ( 'NONE', ( #9861 ), #394, .F. ) ;
#623 = FILL_AREA_STYLE ('',( #9083 ) ) ;
#624 = ORIENTED_EDGE ( 'NONE', *, *, #2970, .T. ) ;
#625 = CARTESIAN_POINT ( 'NONE',  ( -976.0610374937396045, 42.74778062430040393, -141.4553492942756634 ) ) ;
#626 = EDGE_LOOP ( 'NONE', ( #6311, #2844 ) ) ;
#627 = PRODUCT_DEFINITION_SHAPE ( 'NONE', 'NONE',  #12253 ) ;
#628 = ORIENTED_EDGE ( 'NONE', *, *, #11249, .F. ) ;
#629 = AXIS2_PLACEMENT_3D ( 'NONE', #5807, #4770, #10387 ) ;
#630 = CARTESIAN_POINT ( 'NONE',  ( -21.06735260060543879, 180.9331586078316150, -126.2486801514333905 ) ) ;
#631 = ORIENTED_EDGE ( 'NONE', *, *, #733, .T. ) ;
#632 = CARTESIAN_POINT ( 'NONE',  ( -380.5094386830780877, 64.38196187857104746, -134.1524419411843212 ) ) ;
#633 = CARTESIAN_POINT ( 'NONE',  ( -29.99999999999998579, -9.213203435596451385, -126.4213562373092685 ) ) ;
#634 = ORIENTED_EDGE ( 'NONE', *, *, #105, .F. ) ;
#635 = EDGE_CURVE ( 'NONE', #11444, #3617, #5553, .T. ) ;
#636 = DIRECTION ( 'NONE',  ( -1.186840563529527301E-16, 1.000000000000000000, -0.000000000000000000 ) ) ;
#637 = EDGE_LOOP ( 'NONE', ( #8862, #9287, #8745, #1050 ) ) ;
#638 = CIRCLE ( 'NONE', #2031, 1.000000000000000888 ) ;
#639 = EDGE_CURVE ( 'NONE', #5893, #11020, #8714, .T. ) ;
#640 = DIRECTION ( 'NONE',  ( 0.000000000000000000, 1.000000000000000000, 0.000000000000000000 ) ) ;
#641 = CARTESIAN_POINT ( 'NONE',  ( 0.8038475772933552088, -5.196152422706605378, 8.999999999999998224 ) ) ;
#642 = DIRECTION ( 'NONE',  ( 1.000000000000000000, 0.000000000000000000, 0.000000000000000000 ) ) ;
#643 = CARTESIAN_POINT ( 'NONE',  ( -1065.000000000006139, 76.10956187831460795, -95.06748246948023962 ) ) ;
#644 = DIRECTION ( 'NONE',  ( 0.000000000000000000, 1.000000000000000000, 0.000000000000000000 ) ) ;
#645 = DIRECTION ( 'NONE',  ( 0.000000000000000000, 0.000000000000000000, 1.000000000000000000 ) ) ;
#646 = CIRCLE ( 'NONE', #1249, 11.50000000000003730 ) ;
#647 = VERTEX_POINT ( 'NONE', #1446 ) ;
#648 = CARTESIAN_POINT ( 'NONE',  ( -379.7887390581964837, 110.4014878146373633, -134.3428354745942102 ) ) ;
#649 = PLANE ( 'NONE',  #9390 ) ;
#650 = EDGE_LOOP ( 'NONE', ( #11783, #7128, #2797, #3359 ) ) ;
#651 = EDGE_CURVE ( 'NONE', #6732, #6027, #3151, .T. ) ;
#652 = CARTESIAN_POINT ( 'NONE',  ( -59.99999999999998579, -9.213203435596451385, -126.4213562373090696 ) ) ;
#653 = CARTESIAN_POINT ( 'NONE',  ( -1012.828629370415570, 79.69572830938430741, -95.06748246948046699 ) ) ;
#654 = EDGE_CURVE ( 'NONE', #2078, #6153, #6149, .T. ) ;
#655 = CARTESIAN_POINT ( 'NONE',  ( 0.1469846612282483256, 8.891930899535424260, 2.598723904613015723 ) ) ;
#656 = DIRECTION ( 'NONE',  ( -0.000000000000000000, -1.000000000000000000, -0.000000000000000000 ) ) ;
#657 = LINE ( 'NONE', #9378, #2240 ) ;
#658 = CARTESIAN_POINT ( 'NONE',  ( -828.3259789886573117, 76.46577308275197993, -105.4592182070448416 ) ) ;
#659 = CARTESIAN_POINT ( 'NONE',  ( -20.73244433232022033, 180.6366558386295935, -123.3579215951269248 ) ) ;
#660 = CARTESIAN_POINT ( 'NONE',  ( -126.4213562373094959, 0.000000000000000000, 7.500000000000036415 ) ) ;
#661 = AXIS2_PLACEMENT_3D ( 'NONE', #11295, #2830, #6599 ) ;
#662 = LINE ( 'NONE', #4437, #1336 ) ;
#663 = CARTESIAN_POINT ( 'NONE',  ( 1.874378101782966050E-12, 163.9999999999999716, 53.57864376269051832 ) ) ;
#664 = ITEM_DEFINED_TRANSFORMATION ( 'NONE', 'NONE', #6440,  #11957 ) ;
#665 = DIRECTION ( 'NONE',  ( 0.7071067811865473507, 0.000000000000000000, -0.7071067811865477948 ) ) ;
#666 = EDGE_LOOP ( 'NONE', ( #1393, #6344, #2255, #9869 ) ) ;
#667 = CARTESIAN_POINT ( 'NONE',  ( -126.4213562373094959, -6.000000000000000000, -7.499999999999990230 ) ) ;
#668 = CARTESIAN_POINT ( 'NONE',  ( -1065.000000000007731, 112.0000000000007105, -122.7172756069790438 ) ) ;
#669 = DIRECTION ( 'NONE',  ( 0.000000000000000000, 0.000000000000000000, -1.000000000000000000 ) ) ;
#670 = FACE_OUTER_BOUND ( 'NONE', #424, .T. ) ;
#671 = DIRECTION ( 'NONE',  ( 0.000000000000000000, 0.000000000000000000, 1.000000000000000000 ) ) ;
#672 = AXIS2_PLACEMENT_3D ( 'NONE', #2277, #7090, #6167 ) ;
#673 = AXIS2_PLACEMENT_3D ( 'NONE', #5309, #8235, #11995 ) ;
#674 = CARTESIAN_POINT ( 'NONE',  ( 19.99815408692506580, 181.6905235212389869, -124.9672463342703566 ) ) ;
#675 = ORIENTED_EDGE ( 'NONE', *, *, #9229, .F. ) ;
#676 = ORIENTED_EDGE ( 'NONE', *, *, #11233, .F. ) ;
#677 = CARTESIAN_POINT ( 'NONE',  ( -19.83634048512597658, 179.7265707582143079, -127.2348386560517781 ) ) ;
#678 = CARTESIAN_POINT ( 'NONE',  ( 6.899999999999999467, -10.39230484541326405, 0.000000000000000000 ) ) ;
#679 = CARTESIAN_POINT ( 'NONE',  ( -1061.673215548682947, 86.58918783539726860, -154.2940595301283793 ) ) ;
#680 = CIRCLE ( 'NONE', #10546, 8.999999999999998224 ) ;
#681 = SURFACE_STYLE_FILL_AREA ( #9080 ) ;
#682 = LINE ( 'NONE', #10016, #4219 ) ;
#683 = VECTOR ( 'NONE', #11412, 1000.000000000000000 ) ;
#684 = CARTESIAN_POINT ( 'NONE',  ( -1014.911393615049064, 99.73439156315002663, -152.5758913445290261 ) ) ;
#685 = ORIENTED_EDGE ( 'NONE', *, *, #5256, .T. ) ;
#686 = CARTESIAN_POINT ( 'NONE',  ( 1.387778780781445676E-14, -494.9999999999998863, 126.4213562373094959 ) ) ;
#687 = ORIENTED_EDGE ( 'NONE', *, *, #9653, .F. ) ;
#688 = DIRECTION ( 'NONE',  ( 0.000000000000000000, 0.000000000000000000, -1.000000000000000000 ) ) ;
#689 = CARTESIAN_POINT ( 'NONE',  ( -1065.000000000003638, 87.89043812168645786, -154.2940595301284361 ) ) ;
#690 = SHAPE_REPRESENTATION ( 'Mold for bends', ( #11957 ), #500 ) ;
#691 = ORIENTED_EDGE ( 'NONE', *, *, #2021, .F. ) ;
#692 = ADVANCED_FACE ( 'NONE', ( #4300 ), #5147, .T. ) ;
#693 = CIRCLE ( 'NONE', #7604, 70.00000000000002842 ) ;
#694 = VERTEX_POINT ( 'NONE', #2685 ) ;
#695 = ORIENTED_EDGE ( 'NONE', *, *, #8586, .T. ) ;
#696 = CARTESIAN_POINT ( 'NONE',  ( -373.1983853544816725, 64.95592079649878769, -135.2209821354010728 ) ) ;
#697 = CYLINDRICAL_SURFACE ( 'NONE', #6175, 7.499999999999992895 ) ;
#698 = EDGE_LOOP ( 'NONE', ( #3165, #3081, #2133, #7527, #1551 ) ) ;
#699 = FACE_OUTER_BOUND ( 'NONE', #2730, .T. ) ;
#700 = AXIS2_PLACEMENT_3D ( 'NONE', #10293, #12095, #7515 ) ;
#701 = EDGE_LOOP ( 'NONE', ( #6324, #2440, #6315, #11484 ) ) ;
#702 = CARTESIAN_POINT ( 'NONE',  ( -1065.000000000000682, 52.38665522077219805, -130.5712005305403238 ) ) ;
#703 = DIRECTION ( 'NONE',  ( -0.7071067811865479058, 0.000000000000000000, -0.7071067811865472397 ) ) ;
#704 = ADVANCED_FACE ( 'NONE', ( #5459, #10101 ), #8326, .T. ) ;
#705 = FACE_BOUND ( 'NONE', #3097, .T. ) ;
#706 = CARTESIAN_POINT ( 'NONE',  ( 28.00000000000000000, -492.9999999999998863, -27.99999999999999645 ) ) ;
#707 = DIRECTION ( 'NONE',  ( 0.000000000000000000, -1.000000000000000000, -7.930164461608263644E-17 ) ) ;
#708 = EDGE_CURVE ( 'NONE', #4719, #2602, #5527, .T. ) ;
#709 = AXIS2_PLACEMENT_3D ( 'NONE', #714, #11962, #7449 ) ;
#710 = DIRECTION ( 'NONE',  ( 1.000000000000000000, 0.000000000000000000, 0.000000000000000000 ) ) ;
#711 = DIRECTION ( 'NONE',  ( 0.000000000000000000, 1.000000000000000000, -0.000000000000000000 ) ) ;
#712 = ORIENTED_EDGE ( 'NONE', *, *, #11302, .F. ) ;
#713 = CARTESIAN_POINT ( 'NONE',  ( -21.06729583384051097, 179.4139655881280078, -126.1965993184190040 ) ) ;
#714 = CARTESIAN_POINT ( 'NONE',  ( 59.96826639284478233, -2.000000000000001776, 26.30825463659881791 ) ) ;
#715 = CARTESIAN_POINT ( 'NONE',  ( 4.808665244885994618E-14, -6.000000000000000000, 141.4213562373094817 ) ) ;
#716 = ORIENTED_EDGE ( 'NONE', *, *, #5872, .T. ) ;
#717 = CARTESIAN_POINT ( 'NONE',  ( -853.5732225365160275, 62.99598188221410311, -95.06748246948041015 ) ) ;
#718 = PLANE ( 'NONE',  #10433 ) ;
#719 = CARTESIAN_POINT ( 'NONE',  ( -30.00000000000000000, 139.9999999999999716, -126.4213562373092685 ) ) ;
#720 = VECTOR ( 'NONE', #6752, 1000.000000000000000 ) ;
#721 = DIRECTION ( 'NONE',  ( -1.000000000000000000, -0.000000000000000000, -0.000000000000000000 ) ) ;
#722 = DIRECTION ( 'NONE',  ( 0.000000000000000000, 0.000000000000000000, 1.000000000000000000 ) ) ;
#723 = DIRECTION ( 'NONE',  ( -0.000000000000000000, 1.000000000000000000, 7.930164461608263644E-17 ) ) ;
#724 = EDGE_CURVE ( 'NONE', #3617, #11444, #6728, .T. ) ;
#725 = VERTEX_POINT ( 'NONE', #9236 ) ;
#726 = CARTESIAN_POINT ( 'NONE',  ( -369.8747838094790268, 55.70677269066278825, -126.1647431307883522 ) ) ;
#727 = CONTEXT_DEPENDENT_SHAPE_REPRESENTATION ( #8668, #5952 ) ;
#728 = DIRECTION ( 'NONE',  ( 1.000000000000000000, 0.000000000000000000, 0.000000000000000000 ) ) ;
#729 = VECTOR ( 'NONE', #2030, 1000.000000000000000 ) ;
#730 = EDGE_LOOP ( 'NONE', ( #10708, #628 ) ) ;
#731 = CARTESIAN_POINT ( 'NONE',  ( 1.479627290717497352E-14, 11.99999999999999645, 118.9213562373094817 ) ) ;
#732 = CARTESIAN_POINT ( 'NONE',  ( -1017.810720698610226, 119.7719591276204625, -122.7172756069789017 ) ) ;
#733 = EDGE_CURVE ( 'NONE', #10254, #9573, #1405, .T. ) ;
#734 = CARTESIAN_POINT ( 'NONE',  ( 45.53315400109643463, 0.000000000000000000, -237.8419396193597208 ) ) ;
#735 = DIRECTION ( 'NONE',  ( 0.000000000000000000, 1.000000000000000000, -0.000000000000000000 ) ) ;
#736 = CARTESIAN_POINT ( 'NONE',  ( 154.5043356068769071, 12.00000000000000000, -102.0666613060171386 ) ) ;
#737 = ORIENTED_EDGE ( 'NONE', *, *, #10086, .T. ) ;
#738 = CONICAL_SURFACE ( 'NONE', #4100, 9.000000000000000000, 1.047197551196600296 ) ;
#739 = VERTEX_POINT ( 'NONE', #4550 ) ;
#740 = EDGE_CURVE ( 'NONE', #4344, #2611, #2200, .T. ) ;
#741 = DIRECTION ( 'NONE',  ( 1.000000000000000000, 1.486905836551548832E-16, -0.000000000000000000 ) ) ;
#742 = CARTESIAN_POINT ( 'NONE',  ( 126.4213562373094959, -6.000000000000000000, -6.938893903907228378E-15 ) ) ;
#743 = CARTESIAN_POINT ( 'NONE',  ( -994.8066578865465317, 80.00401887192411721, -154.8742214401228523 ) ) ;
#744 = CARTESIAN_POINT ( 'NONE',  ( -828.5731535248166892, 77.06390383656801646, -144.0645491675088294 ) ) ;
#745 = CARTESIAN_POINT ( 'NONE',  ( 0.5584673446549162090, 9.967293815311100147, -0.7361406979141390527 ) ) ;
#746 = CARTESIAN_POINT ( 'NONE',  ( 0.3570196857253447043, 6.047589086024988347, -7.525268439705680379 ) ) ;
#747 = CARTESIAN_POINT ( 'NONE',  ( -794.9999999999980673, 87.89043812168634418, -154.2940595301278961 ) ) ;
#748 = ORIENTED_EDGE ( 'NONE', *, *, #9825, .T. ) ;
#749 = DIRECTION ( 'NONE',  ( 0.000000000000000000, 0.000000000000000000, -1.000000000000000000 ) ) ;
#750 = CARTESIAN_POINT ( 'NONE',  ( -20.00000000000000000, 197.0000000000000000, -124.6807709998038405 ) ) ;
#751 = STYLED_ITEM ( 'NONE', ( #7990 ), #8008 ) ;
#752 =( LENGTH_UNIT ( ) NAMED_UNIT ( * ) SI_UNIT ( .MILLI., .METRE. ) );
#753 = EDGE_LOOP ( 'NONE', ( #7953, #4531, #9259, #7729, #4093, #3852, #8510, #4536, #872, #2326 ) ) ;
#754 = CARTESIAN_POINT ( 'NONE',  ( -1065.000000000004320, 98.77454568802519930, -149.7857175106631189 ) ) ;
#755 = DIRECTION ( 'NONE',  ( -0.000000000000000000, 1.000000000000000000, -0.000000000000000000 ) ) ;
#756 = CARTESIAN_POINT ( 'NONE',  ( -1047.392513188124212, 70.23666496464454667, -154.2940595301285214 ) ) ;
#757 = CARTESIAN_POINT ( 'NONE',  ( 19.83551131833741010, 179.7633983601342038, -127.2411838750873727 ) ) ;
#758 = ORIENTED_EDGE ( 'NONE', *, *, #1083, .F. ) ;
#759 = VERTEX_POINT ( 'NONE', #7445 ) ;
#760 = AXIS2_PLACEMENT_3D ( 'NONE', #9887, #5181, #11805 ) ;
#761 = LINE ( 'NONE', #10215, #10128 ) ;
#762 = DIRECTION ( 'NONE',  ( 0.000000000000000000, 1.000000000000000000, 0.000000000000000000 ) ) ;
#763 = DIRECTION ( 'NONE',  ( -0.000000000000000000, -1.000000000000000000, -0.000000000000000000 ) ) ;
#764 = CARTESIAN_POINT ( 'NONE',  ( -817.4144546772251942, 30.82543593413060279, -136.2353035311987242 ) ) ;
#765 = ORIENTED_EDGE ( 'NONE', *, *, #11667, .F. ) ;
#766 = DIRECTION ( 'NONE',  ( 0.000000000000000000, 0.000000000000000000, -1.000000000000000000 ) ) ;
#767 = CARTESIAN_POINT ( 'NONE',  ( -373.7506463163484796, 67.50546400631965582, -138.5607443211070802 ) ) ;
#768 = CARTESIAN_POINT ( 'NONE',  ( -19.87519864879851994, 178.8871479037923393, -126.9115732480538838 ) ) ;
#769 = PLANE ( 'NONE',  #3066 ) ;
#770 =( BOUNDED_SURFACE ( )  B_SPLINE_SURFACE ( 3, 2, ( 
 ( #7122, #2418, #6198 ),
 ( #9783, #2308, #9966 ),
 ( #6078, #8742, #659 ),
 ( #4630, #9252, #12035 ),
 ( #4435, #11044, #2570 ),
 ( #795, #4563, #923 ),
 ( #8340, #4499, #8410 ),
 ( #2770, #1648, #11178 ),
 ( #8211, #9122, #11245 ),
 ( #11973, #3548, #3689 ),
 ( #12104, #12172, #2702 ),
 ( #5409, #9317, #7337 ),
 ( #3613, #862, #7404 ),
 ( #6473, #11109, #3491 ),
 ( #7276, #6341, #10116 ),
 ( #10247, #2631, #1842 ),
 ( #6410, #1782, #7465 ),
 ( #5545, #6534, #10302 ),
 ( #5606, #9383, #4696 ),
 ( #10608, #11354, #7646 ),
 ( #3810, #10544, #8576 ),
 ( #9441, #10489, #4918 ),
 ( #8700, #100, #978 ),
 ( #3874, #9680, #9559 ),
 ( #7582, #2953, #274 ),
 ( #3998, #6715, #2022 ),
 ( #1105, #1218, #8639 ),
 ( #5911, #2146, #2091 ),
 ( #8758, #151, #9619 ),
 ( #7766, #4065, #5460 ) ),
 .UNSPECIFIED., .F., .F., .F. ) 
 B_SPLINE_SURFACE_WITH_KNOTS ( ( 4, 2, 2, 2, 2, 2, 2, 2, 2, 2, 2, 2, 2, 2, 4 ),
 ( 3, 3 ),
 ( 0.007888614278243437361, 0.008874691063023869633, 0.009367729455414086637, 0.009860767847804301905, 0.01035380624019451891, 0.01084684463258473591, 0.01133988302497495118, 0.01183292141736516818, 0.01281899820214560046, 0.01331203659453581746, 0.01380507498692603446, 0.01429811337931624973, 0.01479115177170646674, 0.01528419016409668374, 0.01577722855648689901 ),
 ( 0.000000000000000000, 1.000000000000000000 ),
 .UNSPECIFIED. ) 
 GEOMETRIC_REPRESENTATION_ITEM ( )  RATIONAL_B_SPLINE_SURFACE ( (
 ( 1.000000000000000000, 0.7778924984312529656, 1.000000000000000000),
 ( 1.000000000000000000, 0.7847112435279847142, 1.000000000000000000),
 ( 1.000000000000000000, 0.7894485421771765266, 1.000000000000000000),
 ( 1.000000000000000000, 0.7926414855251958658, 1.000000000000000000),
 ( 1.000000000000000000, 0.7930469064958857173, 1.000000000000000000),
 ( 1.000000000000000000, 0.7925074991235926403, 1.000000000000000000),
 ( 1.000000000000000000, 0.7915770372355392936, 1.000000000000000000),
 ( 1.000000000000000000, 0.7883898363194743464, 1.000000000000000000),
 ( 1.000000000000000000, 0.7861853387937841608, 1.000000000000000000),
 ( 1.000000000000000000, 0.7806815604416567078, 1.000000000000000000),
 ( 1.000000000000000000, 0.7773361016722152295, 1.000000000000000000),
 ( 1.000000000000000000, 0.7698701636707948603, 1.000000000000000000),
 ( 1.000000000000000000, 0.7657526702509508398, 1.000000000000000000),
 ( 1.000000000000000000, 0.7568812398704235500, 1.000000000000000000),
 ( 1.000000000000000000, 0.7521322257284934754, 1.000000000000000000),
 ( 1.000000000000000000, 0.7377220824064392168, 1.000000000000000000),
 ( 1.000000000000000000, 0.7275566802060602356, 1.000000000000000000),
 ( 1.000000000000000000, 0.7135779984947178134, 1.000000000000000000),
 ( 1.000000000000000000, 0.7090467312072497030, 1.000000000000000000),
 ( 1.000000000000000000, 0.7006183237057392876, 1.000000000000000000),
 ( 1.000000000000000000, 0.6967528866742972449, 1.000000000000000000),
 ( 1.000000000000000000, 0.6897151435478420245, 1.000000000000000000),
 ( 1.000000000000000000, 0.6865208713865151857, 1.000000000000000000),
 ( 1.000000000000000000, 0.6810351634549236532, 1.000000000000000000),
 ( 1.000000000000000000, 0.6787116622188523740, 1.000000000000000000),
 ( 1.000000000000000000, 0.6747765002012137137, 1.000000000000000000),
 ( 1.000000000000000000, 0.6731806124592021323, 1.000000000000000000),
 ( 1.000000000000000000, 0.6706618708365198467, 1.000000000000000000),
 ( 1.000000000000000000, 0.6697163794380122104, 1.000000000000000000),
 ( 1.000000000000000000, 0.6689879873414465994, 1.000000000000000000) ) ) 
 REPRESENTATION_ITEM ( '' )  SURFACE ( )  );
#771 = PLANE ( 'NONE',  #1682 ) ;
#772 = DIRECTION ( 'NONE',  ( 1.000000000000000000, 0.000000000000000000, -0.000000000000000000 ) ) ;
#773 = CARTESIAN_POINT ( 'NONE',  ( 19.87268743161337170, 178.9255784920988503, -126.9338343023757290 ) ) ;
#774 = DIRECTION ( 'NONE',  ( 3.061276722312011504E-17, -1.000000000000000000, 0.000000000000000000 ) ) ;
#775 = AXIS2_PLACEMENT_3D ( 'NONE', #5067, #5187, #3271 ) ;
#776 = CARTESIAN_POINT ( 'NONE',  ( -995.4135022096149896, 71.70161378084165449, -95.06748246948046699 ) ) ;
#777 = CARTESIAN_POINT ( 'NONE',  ( 0.000000000000000000, 12.00000000000000000, -89.68077099980401101 ) ) ;
#778 = LINE ( 'NONE', #4551, #2867 ) ;
#779 = CARTESIAN_POINT ( 'NONE',  ( -820.7807412222841776, 82.64141399635654750, -144.6707558958804043 ) ) ;
#780 = ORIENTED_EDGE ( 'NONE', *, *, #4037, .T. ) ;
#781 = DIRECTION ( 'NONE',  ( -0.000000000000000000, 1.000000000000000000, -0.000000000000000000 ) ) ;
#782 = EDGE_CURVE ( 'NONE', #9741, #2455, #10, .T. ) ;
#783 = DIRECTION ( 'NONE',  ( 0.03251933543158296025, 7.479798524539567821E-17, 0.9994711065474020106 ) ) ;
#784 = CARTESIAN_POINT ( 'NONE',  ( -369.8980370199456047, 108.2344238686749520, -123.1401886717858787 ) ) ;
#785 = ORIENTED_EDGE ( 'NONE', *, *, #9267, .F. ) ;
#786 = DIRECTION ( 'NONE',  ( -1.000000000000000000, 0.000000000000000000, 0.000000000000000000 ) ) ;
#787 = VECTOR ( 'NONE', #1857, 1000.000000000000000 ) ;
#789 = EDGE_CURVE ( 'NONE', #11268, #694, #18, .T. ) ;
#788 = CARTESIAN_POINT ( 'NONE',  ( -1062.665377791213132, 57.01990411978262330, -103.3307627799634503 ) ) ;
#790 = DIRECTION ( 'NONE',  ( -0.000000000000000000, 1.000000000000000000, 7.930164461608263644E-17 ) ) ;
#791 = CIRCLE ( 'NONE', #11439, 12.52076803445814690 ) ;
#792 = PLANE ( 'NONE',  #6380 ) ;
#793 = EDGE_CURVE ( 'NONE', #6696, #8838, #10230, .T. ) ;
#794 = CARTESIAN_POINT ( 'NONE',  ( -820.7525053003647599, 74.71879621637245350, -106.0522004026985456 ) ) ;
#795 = CARTESIAN_POINT ( 'NONE',  ( -19.87376422533415266, 179.9397883299151601, -122.4372163154974942 ) ) ;
#796 = DIRECTION ( 'NONE',  ( 0.000000000000000000, 1.000000000000000000, 0.000000000000000000 ) ) ;
#797 = ORIENTED_EDGE ( 'NONE', *, *, #3584, .F. ) ;
#798 = EDGE_LOOP ( 'NONE', ( #9828, #5326 ) ) ;
#799 = DIRECTION ( 'NONE',  ( 0.000000000000000000, 1.000000000000000000, 0.000000000000000000 ) ) ;
#800 = CONTEXT_DEPENDENT_SHAPE_REPRESENTATION ( #1471, #627 ) ;
#801 = CARTESIAN_POINT ( 'NONE',  ( -374.4786324000669424, 91.82513850978268977, -107.1885437437087063 ) ) ;
#802 = ORIENTED_EDGE ( 'NONE', *, *, #5618, .F. ) ;
#803 = CARTESIAN_POINT ( 'NONE',  ( -1021.777026427247165, 118.8177985574657924, -118.7903414690675561 ) ) ;
#804 = CARTESIAN_POINT ( 'NONE',  ( 21.06240745282767435, 180.2041921146315246, -126.4269926335259413 ) ) ;
#805 = DIRECTION ( 'NONE',  ( -1.000000000000000000, 0.000000000000000000, 0.000000000000000000 ) ) ;
#806 = DIRECTION ( 'NONE',  ( 0.000000000000000000, 0.000000000000000000, -1.000000000000000000 ) ) ;
#807 = EDGE_CURVE ( 'NONE', #7831, #11221, #10092, .T. ) ;
#808 = CARTESIAN_POINT ( 'NONE',  ( 19.86936981681406778, 181.4590435457396609, -126.9708661016945257 ) ) ;
#809 = EDGE_LOOP ( 'NONE', ( #4329, #2289, #4115, #6023 ) ) ;
#810 = ORIENTED_EDGE ( 'NONE', *, *, #11144, .T. ) ;
#811 = CARTESIAN_POINT ( 'NONE',  ( 1.387778780781445676E-14, -6.000000000000000000, 126.4213562373094959 ) ) ;
#812 = CARTESIAN_POINT ( 'NONE',  ( 1.561981751485805177E-12, 163.9999999999999716, 31.07864376269052542 ) ) ;
#813 = CARTESIAN_POINT ( 'NONE',  ( -1022.719357623492101, 104.5170332807324769, -149.7857175106632610 ) ) ;
#814 = CARTESIAN_POINT ( 'NONE',  ( -828.3261744505593924, 76.46613818254142814, -143.9024326026600988 ) ) ;
#815 = SURFACE_STYLE_FILL_AREA ( #9277 ) ;
#816 = CARTESIAN_POINT ( 'NONE',  ( 0.5590800469813590468, 5.620102221249812402, -8.265697409064609147 ) ) ;
#817 = CARTESIAN_POINT ( 'NONE',  ( -82.49999999999997158, -9.213203435596451385, -126.4213562373088564 ) ) ;
#818 = VERTEX_POINT ( 'NONE', #8260 ) ;
#819 = CYLINDRICAL_SURFACE ( 'NONE', #3637, 7.500000000000007105 ) ;
#820 = LINE ( 'NONE', #1865, #6878 ) ;
#821 = CARTESIAN_POINT ( 'NONE',  ( -381.5603242327452449, 97.47709203580956228, -137.3647392459991750 ) ) ;
#822 = VERTEX_POINT ( 'NONE', #12019 ) ;
#823 = CARTESIAN_POINT ( 'NONE',  ( -902.8257469293334907, 84.21185948885708683, -154.2940595301280950 ) ) ;
#824 = EDGE_CURVE ( 'NONE', #11283, #7319, #1411, .T. ) ;
#825 = CARTESIAN_POINT ( 'NONE',  ( -1065.000000000003865, 112.0000000000008527, -126.6442663926290493 ) ) ;
#826 = CARTESIAN_POINT ( 'NONE',  ( 19.98066683771208574, 182.6001984525962030, -125.5662099944124748 ) ) ;
#827 = ORIENTED_EDGE ( 'NONE', *, *, #9947, .T. ) ;
#828 = AXIS2_PLACEMENT_3D ( 'NONE', #6958, #5155, #8814 ) ;
#829 = ORIENTED_EDGE ( 'NONE', *, *, #8003, .T. ) ;
#830 = CARTESIAN_POINT ( 'NONE',  ( -19.99331759212207515, 182.5955720455716573, -124.1413515841623649 ) ) ;
#831 = CARTESIAN_POINT ( 'NONE',  ( -828.6675604493494802, 77.37337224769281363, -105.2204629476323277 ) ) ;
#832 = ORIENTED_EDGE ( 'NONE', *, *, #4675, .F. ) ;
#833 = CARTESIAN_POINT ( 'NONE',  ( -373.5661612086483387, 66.59315941246912018, -137.5313104353387530 ) ) ;
#834 = DIRECTION ( 'NONE',  ( 0.000000000000000000, 0.000000000000000000, 1.000000000000000000 ) ) ;
#835 = AXIS2_PLACEMENT_3D ( 'NONE', #1633, #2618, #6521 ) ;
#836 = DIRECTION ( 'NONE',  ( -1.000000000000000000, 0.000000000000000000, 0.000000000000000000 ) ) ;
#837 = ORIENTED_EDGE ( 'NONE', *, *, #12209, .F. ) ;
#838 = CARTESIAN_POINT ( 'NONE',  ( 154.5043356068769071, 12.00000000000000000, -102.0666613060171386 ) ) ;
#839 = AXIS2_PLACEMENT_3D ( 'NONE', #11119, #4323, #8349 ) ;
#840 = PLANE ( 'NONE',  #2310 ) ;
#841 = CARTESIAN_POINT ( 'NONE',  ( 35.00000000000000000, 82.00000000000071054, -124.6807709998040394 ) ) ;
#842 = CARTESIAN_POINT ( 'NONE',  ( -1023.860074334734577, 85.97273905232950142, -94.48732055948609343 ) ) ;
#843 = CARTESIAN_POINT ( 'NONE',  ( -19.03136272649511085, 180.2041921146316668, -134.6807709998038547 ) ) ;
#844 = DIRECTION ( 'NONE',  ( -0.7071067811865526798, 8.659560562354869996E-17, -0.7071067811865423547 ) ) ;
#845 = DIRECTION ( 'NONE',  ( 2.040851148208007875E-17, -1.000000000000000000, -0.000000000000000000 ) ) ;
#846 = VECTOR ( 'NONE', #8160, 1000.000000000000000 ) ;
#847 = CIRCLE ( 'NONE', #2211, 7.500000000000007105 ) ;
#848 = AXIS2_PLACEMENT_3D ( 'NONE', #5293, #9070, #604 ) ;
#849 = ORIENTED_EDGE ( 'NONE', *, *, #4932, .F. ) ;
#850 = DIRECTION ( 'NONE',  ( 1.000000000000000000, 0.000000000000000000, 0.000000000000000000 ) ) ;
#851 = CARTESIAN_POINT ( 'NONE',  ( -370.4631672708575252, 106.7912974028927806, -114.8027370444668662 ) ) ;
#852 = ORIENTED_EDGE ( 'NONE', *, *, #4369, .F. ) ;
#853 = CARTESIAN_POINT ( 'NONE',  ( -902.2382941300801349, 66.55116351576566558, -103.3307627799636066 ) ) ;
#854 = DIRECTION ( 'NONE',  ( -0.000000000000000000, 1.000000000000000000, 7.930164461608263644E-17 ) ) ;
#855 = CARTESIAN_POINT ( 'NONE',  ( -187.5000000000000000, 24.00000000000001421, -126.4213562373082453 ) ) ;
#856 = DIRECTION ( 'NONE',  ( 0.000000000000000000, 0.000000000000000000, 1.000000000000000000 ) ) ;
#857 =( REPRESENTATION_RELATIONSHIP ('NONE','NONE', #12149, #1102 ) REPRESENTATION_RELATIONSHIP_WITH_TRANSFORMATION ( #8345 )SHAPE_REPRESENTATION_RELATIONSHIP( ) );
#858 = CARTESIAN_POINT ( 'NONE',  ( 141.4213562373095101, -494.9999999999998863, -1.508194112741312283E-14 ) ) ;
#859 = AXIS2_PLACEMENT_3D ( 'NONE', #211, #8634, #7891 ) ;
#860 = EDGE_CURVE ( 'NONE', #3022, #6536, #1699, .T. ) ;
#861 = CARTESIAN_POINT ( 'NONE',  ( -823.4970567115291260, 73.67398878492905112, -106.4962298347509631 ) ) ;
#862 = CARTESIAN_POINT ( 'NONE',  ( -19.98517529853678809, 179.0632710820790976, -123.7013734869633197 ) ) ;
#863 = CARTESIAN_POINT ( 'NONE',  ( -826.3639150177590409, 74.35254223074673519, -143.1619793993633323 ) ) ;
#864 = VERTEX_POINT ( 'NONE', #11160 ) ;
#865 = CARTESIAN_POINT ( 'NONE',  ( -372.8682051073146226, 64.83784294256510350, -147.4127590854037635 ) ) ;
#866 = CARTESIAN_POINT ( 'NONE',  ( -384.1845455826150442, 89.69765040021600555, -106.1749927342177102 ) ) ;
#867 = VERTEX_POINT ( 'NONE', #1574 ) ;
#868 = CARTESIAN_POINT ( 'NONE',  ( -1018.154501869011938, 114.3413228342526082, -107.9061927053323870 ) ) ;
#869 = DIRECTION ( 'NONE',  ( 1.000000000000000000, -1.876626137810916309E-30, 2.081668171172161734E-17 ) ) ;
#870 = CARTESIAN_POINT ( 'NONE',  ( 19.99218703114167539, 182.5822718396941582, -124.1010742661679274 ) ) ;
#871 = AXIS2_PLACEMENT_3D ( 'NONE', #2824, #2567, #2628 ) ;
#872 = ORIENTED_EDGE ( 'NONE', *, *, #898, .T. ) ;
#873 = CARTESIAN_POINT ( 'NONE',  ( -991.5701548301636876, 122.8678427087060214, -124.6807709998040536 ) ) ;
#874 = EDGE_CURVE ( 'NONE', #6680, #11382, #2755, .T. ) ;
#875 = CARTESIAN_POINT ( 'NONE',  ( -154.5043356068770493, 12.00000000000000000, -94.56666130601601594 ) ) ;
#876 = LINE ( 'NONE', #8424, #1553 ) ;
#877 = CARTESIAN_POINT ( 'NONE',  ( -1014.632462699976486, 105.5176738732105690, -149.7857175106636589 ) ) ;
#878 = CARTESIAN_POINT ( 'NONE',  ( -369.9630775916107268, 108.0732521340322876, -120.6787736983387163 ) ) ;
#879 = DIRECTION ( 'NONE',  ( 0.000000000000000000, 0.000000000000000000, 1.000000000000000000 ) ) ;
#880 = CARTESIAN_POINT ( 'NONE',  ( 0.1469846612282468268, 6.696526368584462041, -6.401276095386994491 ) ) ;
#881 = CARTESIAN_POINT ( 'NONE',  ( 2.186774452080127126E-12, 0.000000000000000000, 83.57864376269050410 ) ) ;
#882 = VERTEX_POINT ( 'NONE', #9106 ) ;
#883 = DIRECTION ( 'NONE',  ( 0.000000000000000000, 0.000000000000000000, -1.000000000000000000 ) ) ;
#884 = CIRCLE ( 'NONE', #7177, 20.00000000000017053 ) ;
#885 = CIRCLE ( 'NONE', #12132, 7.500000000000007105 ) ;
#886 = ORIENTED_EDGE ( 'NONE', *, *, #1701, .F. ) ;
#887 = CARTESIAN_POINT ( 'NONE',  ( -853.5732225365131853, 62.99598188221416706, -154.2940595301278108 ) ) ;
#888 = CARTESIAN_POINT ( 'NONE',  ( 19.96426536123311735, 182.4767232793243181, -125.8798892712007245 ) ) ;
#889 = ORIENTED_EDGE ( 'NONE', *, *, #11610, .F. ) ;
#890 = EDGE_LOOP ( 'NONE', ( #10634, #2205 ) ) ;
#891 = AXIS2_PLACEMENT_3D ( 'NONE', #6379, #6445, #10149 ) ;
#892 = AXIS2_PLACEMENT_3D ( 'NONE', #10290, #12162, #2817 ) ;
#893 = DIRECTION ( 'NONE',  ( 0.000000000000000000, 1.000000000000000000, 0.000000000000000000 ) ) ;
#894 = CARTESIAN_POINT ( 'NONE',  ( -20.00092085174054546, 181.7296212712162173, -124.7139161294905136 ) ) ;
#895 = AXIS2_PLACEMENT_3D ( 'NONE', #268, #10484, #4853 ) ;
#896 = CARTESIAN_POINT ( 'NONE',  ( -826.3665850287353578, 74.35417337301176133, -106.1988918232332821 ) ) ;
#897 = EDGE_LOOP ( 'NONE', ( #5030, #10337, #10470, #5661 ) ) ;
#898 = EDGE_CURVE ( 'NONE', #2093, #11305, #6146, .T. ) ;
#899 = CARTESIAN_POINT ( 'NONE',  ( -374.1450238171013893, 69.75518729278782359, -140.5780087988560183 ) ) ;
#900 = CARTESIAN_POINT ( 'NONE',  ( 0.000000000000000000, 152.0000000000000284, -126.4213562373094959 ) ) ;
#901 = DIRECTION ( 'NONE',  ( 0.000000000000000000, 0.000000000000000000, 1.000000000000000000 ) ) ;
#902 = B_SPLINE_CURVE_WITH_KNOTS ( 'NONE', 3,
 ( #9879, #8090, #6047, #354, #5288, #4192, #9064, #5173, #11741, #4138, #6972, #11912, #3432, #2454, #5228, #3196, #7094, #1353, #600, #467 ),
 .UNSPECIFIED., .F., .F.,
 ( 4, 1, 1, 1, 2, 1, 1, 1, 2, 2, 2, 2, 4 ),
 ( 0.000000000000000000, 0.04762575996673557022, 0.07143863995010346635, 0.09525151993347125146, 0.1428772799002068217, 0.1647615404280894369, 0.1757036706920307445, 0.1866458009559719411, 0.2085300614838545563, 0.4016963878702066726, 0.4307237013227157574, 0.6771470142487683308, 1.000000000000000000 ),
 .UNSPECIFIED. ) ;
#903 = EDGE_CURVE ( 'NONE', #7035, #9732, #8909, .T. ) ;
#904 = EDGE_CURVE ( 'NONE', #8838, #7471, #2559, .T. ) ;
#905 = AXIS2_PLACEMENT_3D ( 'NONE', #9527, #2866, #1994 ) ;
#906 = CIRCLE ( 'NONE', #10557, 70.00000000000002842 ) ;
#907 = DIRECTION ( 'NONE',  ( 0.000000000000000000, 0.000000000000000000, 1.000000000000000000 ) ) ;
#908 = DIRECTION ( 'NONE',  ( 0.000000000000000000, -1.189524669241239115E-16, 1.000000000000000000 ) ) ;
#909 = CARTESIAN_POINT ( 'NONE',  ( 21.04869859328100290, 178.8069441414488097, -125.4530315734257471 ) ) ;
#910 = CARTESIAN_POINT ( 'NONE',  ( -902.2382941300801349, 66.55116351576566558, -103.3307627799636066 ) ) ;
#911 = FACE_OUTER_BOUND ( 'NONE', #1496, .T. ) ;
#912 = CARTESIAN_POINT ( 'NONE',  ( -901.8785362142587019, 56.55314031071017666, -122.7172756069789017 ) ) ;
#913 = EDGE_CURVE ( 'NONE', #9220, #9416, #3010, .T. ) ;
#914 = AXIS2_PLACEMENT_3D ( 'NONE', #2500, #4427, #1515 ) ;
#915 = VERTEX_POINT ( 'NONE', #5828 ) ;
#916 = CARTESIAN_POINT ( 'NONE',  ( -27.99999999999999645, -492.9999999999998863, -27.99999999999999645 ) ) ;
#917 = CARTESIAN_POINT ( 'NONE',  ( -373.0711960171485657, 98.34294693636040563, -101.1726803376526505 ) ) ;
#918 = VERTEX_POINT ( 'NONE', #2812 ) ;
#919 = CARTESIAN_POINT ( 'NONE',  ( -795.0000000000022737, 65.22545431197607968, -99.57582448894522997 ) ) ;
#920 = CARTESIAN_POINT ( 'NONE',  ( 1.249585401188644101E-12, 0.000000000000000000, 1.078643762690513874 ) ) ;
#921 = DIRECTION ( 'NONE',  ( 0.000000000000000000, -0.9464175275073136717, 0.3229456047493806103 ) ) ;
#922 = CARTESIAN_POINT ( 'NONE',  ( -828.8285638327206470, 78.34605190446892209, -105.0145692953448133 ) ) ;
#923 = CARTESIAN_POINT ( 'NONE',  ( -20.72096896666972299, 180.0455498438134896, -123.3107784691637079 ) ) ;
#924 = LINE ( 'NONE', #5726, #266 ) ;
#925 = EDGE_LOOP ( 'NONE', ( #10478, #7807, #5815, #9444 ) ) ;
#926 = CARTESIAN_POINT ( 'NONE',  ( -21.06240745282767080, 180.2041921146517041, -126.4269926335259413 ) ) ;
#927 = ORIENTED_EDGE ( 'NONE', *, *, #5402, .T. ) ;
#928 = CARTESIAN_POINT ( 'NONE',  ( -1017.963927524554038, 117.4283576114806777, -113.1262384684094968 ) ) ;
#929 = VECTOR ( 'NONE', #3107, 1000.000000000000000 ) ;
#930 = CARTESIAN_POINT ( 'NONE',  ( 1.874378101782966050E-12, -6.000000000000005329, 53.57864376269050410 ) ) ;
#931 = VERTEX_POINT ( 'NONE', #4901 ) ;
#932 = AXIS2_PLACEMENT_3D ( 'NONE', #9914, #5152, #9977 ) ;
#933 = CARTESIAN_POINT ( 'NONE',  ( 35.00000000000000000, 2.428612866367529932E-14, -159.6807709998040252 ) ) ;
#934 = FACE_OUTER_BOUND ( 'NONE', #2126, .T. ) ;
#935 = CARTESIAN_POINT ( 'NONE',  ( -903.0443340174343803, 90.92133391050434454, -154.8742214401225112 ) ) ;
#936 = DIRECTION ( 'NONE',  ( -0.000000000000000000, -1.000000000000000000, -1.757987137413040192E-14 ) ) ;
#937 = DIRECTION ( 'NONE',  ( -1.000000000000000000, -0.000000000000000000, 0.000000000000000000 ) ) ;
#938 = ORIENTED_EDGE ( 'NONE', *, *, #10249, .F. ) ;
#939 = DIRECTION ( 'NONE',  ( -0.000000000000000000, -1.000000000000000000, -0.000000000000000000 ) ) ;
#940 = CARTESIAN_POINT ( 'NONE',  ( -1045.864486809339269, 115.5688325305735162, -126.6442663926293477 ) ) ;
#941 = EDGE_CURVE ( 'NONE', #178, #9730, #11411, .T. ) ;
#942 = EDGE_LOOP ( 'NONE', ( #4491, #737, #7354, #4686, #5672 ) ) ;
#943 = CARTESIAN_POINT ( 'NONE',  ( -1061.673215548682947, 86.58918783539726860, -154.2940595301283793 ) ) ;
#944 = EDGE_CURVE ( 'NONE', #3591, #6687, #10892, .T. ) ;
#945 = VECTOR ( 'NONE', #10974, 1000.000000000000000 ) ;
#946 = ORIENTED_EDGE ( 'NONE', *, *, #12081, .T. ) ;
#947 = ORIENTED_EDGE ( 'NONE', *, *, #1332, .F. ) ;
#948 = EDGE_CURVE ( 'NONE', #11949, #8436, #3579, .T. ) ;
#949 = CARTESIAN_POINT ( 'NONE',  ( -828.8285638327243987, 78.67432280806561096, -104.9592124606052863 ) ) ;
#950 = CARTESIAN_POINT ( 'NONE',  ( -1013.844210246968942, 57.79547239392000790, -141.4553492942758908 ) ) ;
#951 = ORIENTED_EDGE ( 'NONE', *, *, #3247, .T. ) ;
#952 = MECHANICAL_DESIGN_GEOMETRIC_PRESENTATION_REPRESENTATION (  '', ( #1937 ), #2926 ) ;
#953 = CARTESIAN_POINT ( 'NONE',  ( -374.9534812425817449, 79.41157780634799224, -154.5387344296071319 ) ) ;
#954 = CARTESIAN_POINT ( 'NONE',  ( 87.04832655144112152, 12.00000000000000000, -225.4289243767383368 ) ) ;
#955 = B_SPLINE_CURVE_WITH_KNOTS ( 'NONE', 3,
 ( #11864, #5021, #2525, #4106, #10938, #8230, #9138, #11926, #3379, #10652, #7171, #10998, #5360, #612, #1542, #5303, #3167, #6016 ),
 .UNSPECIFIED., .F., .F.,
 ( 4, 2, 2, 2, 2, 2, 2, 2, 4 ),
 ( 0.007924218878882885106, 0.008564103707084826447, 0.009203988535286766054, 0.009843873363488707395, 0.01048375819169064874, 0.01112364301989258834, 0.01176352784809452968, 0.01240341267629646929, 0.01304329750449841063 ),
 .UNSPECIFIED. ) ;
#956 = DIRECTION ( 'NONE',  ( 0.000000000000000000, 0.000000000000000000, 1.000000000000000000 ) ) ;
#957 = VERTEX_POINT ( 'NONE', #3052 ) ;
#958 = CIRCLE ( 'NONE', #351, 7.500000000000007105 ) ;
#959 = EDGE_CURVE ( 'NONE', #6830, #3523, #9629, .T. ) ;
#960 = CARTESIAN_POINT ( 'NONE',  ( -97.49999999999998579, -9.213203435596451385, -126.4213562373088564 ) ) ;
#961 = DIRECTION ( 'NONE',  ( 0.000000000000000000, 1.000000000000000000, 0.000000000000000000 ) ) ;
#962 = CARTESIAN_POINT ( 'NONE',  ( -1038.401083800584274, 57.54275223462379074, -99.57582448894500260 ) ) ;
#963 = CARTESIAN_POINT ( 'NONE',  ( -828.3277261219677712, 80.87986238895041424, -104.7098637035480238 ) ) ;
#964 = CARTESIAN_POINT ( 'NONE',  ( -1038.708781889657075, 41.03774456592552156, -130.5712005305402670 ) ) ;
#965 = VECTOR ( 'NONE', #2823, 1000.000000000000000 ) ;
#966 = VERTEX_POINT ( 'NONE', #80 ) ;
#967 = VECTOR ( 'NONE', #6992, 999.9999999999998863 ) ;
#968 = CARTESIAN_POINT ( 'NONE',  ( 27.10787553788151172, 180.2041921146317520, -137.3302880892914288 ) ) ;
#969 =( LENGTH_UNIT ( ) NAMED_UNIT ( * ) SI_UNIT ( .MILLI., .METRE. ) );
#970 = CARTESIAN_POINT ( 'NONE',  ( -369.9251870295186677, 108.1672116062914029, -127.1279719650820255 ) ) ;
#971 = ORIENTED_EDGE ( 'NONE', *, *, #9425, .T. ) ;
#972 = CARTESIAN_POINT ( 'NONE',  ( -956.9243412622536198, 54.10650223846825924, -107.9061927053324439 ) ) ;
#973 = DIRECTION ( 'NONE',  ( -8.163404592832030268E-17, 1.000000000000000000, -0.000000000000000000 ) ) ;
#974 = FACE_OUTER_BOUND ( 'NONE', #10045, .T. ) ;
#975 = ADVANCED_FACE ( 'NONE', ( #911 ), #3858, .T. ) ;
#976 = AXIS2_PLACEMENT_3D ( 'NONE', #9716, #10818, #2236 ) ;
#977 = DIRECTION ( 'NONE',  ( 1.000000000000000000, 0.000000000000000000, 0.000000000000000000 ) ) ;
#978 = CARTESIAN_POINT ( 'NONE',  ( -21.04715153834148467, 178.7974658297258372, -125.4275705862621066 ) ) ;
#979 = CARTESIAN_POINT ( 'NONE',  ( -150.0000000000000000, -9.213203435596451385, -126.4213562373084301 ) ) ;
#980 = ORIENTED_EDGE ( 'NONE', *, *, #11838, .T. ) ;
#981 = CARTESIAN_POINT ( 'NONE',  ( -210.0000000000000000, -9.213203435596478030, -126.4213562373080180 ) ) ;
#982 =( GEOMETRIC_REPRESENTATION_CONTEXT ( 3 ) GLOBAL_UNCERTAINTY_ASSIGNED_CONTEXT ( ( #7947 ) ) GLOBAL_UNIT_ASSIGNED_CONTEXT ( ( #4651, #9582, #8536 ) ) REPRESENTATION_CONTEXT ( 'NONE', 'WORKASPACE' ) );
#983 = AXIS2_PLACEMENT_3D ( 'NONE', #1406, #8087, #9811 ) ;
#984 = ORIENTED_EDGE ( 'NONE', *, *, #5781, .T. ) ;
#985 = CARTESIAN_POINT ( 'NONE',  ( -1046.261572611724432, 104.4651992465225447, -103.3307627799636208 ) ) ;
#986 = CARTESIAN_POINT ( 'NONE',  ( -35.00000000000000000, 81.99999999999998579, 190.3192290001959748 ) ) ;
#987 = DIRECTION ( 'NONE',  ( -0.000000000000000000, 1.000000000000000000, 7.930164461608263644E-17 ) ) ;
#988 = EDGE_CURVE ( 'NONE', #6938, #1262, #2405, .T. ) ;
#989 = CARTESIAN_POINT ( 'NONE',  ( -1045.864486809339724, 115.5688325305733741, -124.6807709998043663 ) ) ;
#990 = TOROIDAL_SURFACE ( 'NONE', #6899, 10.00000000000002487, 1.499999999999998002 ) ;
#991 = ORIENTED_EDGE ( 'NONE', *, *, #7995, .F. ) ;
#992 = CARTESIAN_POINT ( 'NONE',  ( 2.187692937179487324E-12, 0.000000000000000000, 76.07864376269048989 ) ) ;
#993 = DIRECTION ( 'NONE',  ( -1.000000000000000000, -0.000000000000000000, -0.000000000000000000 ) ) ;
#994 = DIRECTION ( 'NONE',  ( 0.000000000000000000, -1.000000000000000000, 0.000000000000000000 ) ) ;
#995 = CARTESIAN_POINT ( 'NONE',  ( -795.0000000000006821, 98.77454568802552615, -149.7857175106634884 ) ) ;
#996 = DIRECTION ( 'NONE',  ( -8.163404592832030268E-17, 1.000000000000000000, -0.000000000000000000 ) ) ;
#997 = CARTESIAN_POINT ( 'NONE',  ( 6.247927005943220505E-13, -6.000000000000005329, -66.42135623730949590 ) ) ;
#998 = ORIENTED_EDGE ( 'NONE', *, *, #33, .F. ) ;
#999 = CARTESIAN_POINT ( 'NONE',  ( -373.1039460868908009, 99.45530451436835051, -134.6103044504524462 ) ) ;
#1000 = VERTEX_POINT ( 'NONE', #10591 ) ;
#1001 = CARTESIAN_POINT ( 'NONE',  ( -1060.773655115453948, 112.4236047030759238, -130.5712005305406080 ) ) ;
#1002 = CARTESIAN_POINT ( 'NONE',  ( -1060.756016675584760, 112.8516620848307355, -126.6442663926292056 ) ) ;
#1003 = FACE_BOUND ( 'NONE', #3356, .T. ) ;
#1004 = ORIENTED_EDGE ( 'NONE', *, *, #1417, .F. ) ;
#1005 = ORIENTED_EDGE ( 'NONE', *, *, #566, .F. ) ;
#1006 = CARTESIAN_POINT ( 'NONE',  ( 20.86846003075320866, 178.9597637446144631, -123.9944097082106396 ) ) ;
#1007 = EDGE_CURVE ( 'NONE', #6027, #2717, #3007, .T. ) ;
#1008 = LINE ( 'NONE', #3962, #3248 ) ;
#1009 = CARTESIAN_POINT ( 'NONE',  ( -20.00222207760924320, 182.7106143631367559, -124.6033207595390593 ) ) ;
#1010 = CARTESIAN_POINT ( 'NONE',  ( -827.8285638327242850, 78.67432280806536937, -90.68077099980378364 ) ) ;
#1011 = FACE_BOUND ( 'NONE', #10350, .T. ) ;
#1012 = ORIENTED_EDGE ( 'NONE', *, *, #12147, .T. ) ;
#1013 = CARTESIAN_POINT ( 'NONE',  ( -373.1558531919824873, 65.98301015230569533, -148.5292176372442725 ) ) ;
#1014 = EDGE_CURVE ( 'NONE', #11690, #11084, #1599, .T. ) ;
#1015 = FACE_OUTER_BOUND ( 'NONE', #7771, .T. ) ;
#1016 = APPLICATION_CONTEXT ( 'automotive_design' ) ;
#1017 = CYLINDRICAL_SURFACE ( 'NONE', #5268, 7.499999999999992895 ) ;
#1018 = AXIS2_PLACEMENT_3D ( 'NONE', #7016, #1338, #5969 ) ;
#1019 = DIRECTION ( 'NONE',  ( -1.000000000000000000, 0.000000000000000000, 0.000000000000000000 ) ) ;
#1020 = CARTESIAN_POINT ( 'NONE',  ( 0.000000000000000000, 12.00000000000000000, -224.6807709998039968 ) ) ;
#1021 = CARTESIAN_POINT ( 'NONE',  ( -1057.299536696272526, 52.76571712355550403, -103.3307627799637487 ) ) ;
#1022 = CYLINDRICAL_SURFACE ( 'NONE', #4880, 7.500000000000007994 ) ;
#1023 = CARTESIAN_POINT ( 'NONE',  ( 0.8038475772931109598, -5.196152422707023710, -9.000000000000001776 ) ) ;
#1024 = DIRECTION ( 'NONE',  ( 0.000000000000000000, 0.000000000000000000, 1.000000000000000000 ) ) ;
#1025 = CARTESIAN_POINT ( 'NONE',  ( -1038.719578313837474, 40.52245044769760085, -126.6442663926297740 ) ) ;
#1026 = EDGE_CURVE ( 'NONE', #5299, #3186, #258, .T. ) ;
#1027 = ORIENTED_EDGE ( 'NONE', *, *, #3586, .T. ) ;
#1028 = ORIENTED_EDGE ( 'NONE', *, *, #10086, .F. ) ;
#1029 = CARTESIAN_POINT ( 'NONE',  ( -826.3405481598703091, 83.00984762678743323, -144.6560901833811670 ) ) ;
#1030 = ADVANCED_FACE ( 'NONE', ( #11648 ), #2322, .T. ) ;
#1031 = APPLICATION_PROTOCOL_DEFINITION ( 'draft international standard', 'automotive_design', 1998, #426 ) ;
#1032 = CARTESIAN_POINT ( 'NONE',  ( -370.7906933011090587, 105.9194442196002797, -112.1115210325544211 ) ) ;
#1033 = EDGE_LOOP ( 'NONE', ( #203, #3266, #1398, #1116 ) ) ;
#1034 = AXIS2_PLACEMENT_3D ( 'NONE', #858, #4628, #3686 ) ;
#1035 = CARTESIAN_POINT ( 'NONE',  ( -1064.999999999999545, 54.10491585757062438, -113.1262384684097668 ) ) ;
#1036 = EDGE_CURVE ( 'NONE', #7665, #6732, #955, .T. ) ;
#1037 = DIRECTION ( 'NONE',  ( -1.000000000000000000, -0.000000000000000000, -0.000000000000000000 ) ) ;
#1038 = CARTESIAN_POINT ( 'NONE',  ( 6.899999999999999467, 8.999999999999998224, 0.000000000000000000 ) ) ;
#1039 = FACE_OUTER_BOUND ( 'NONE', #11944, .T. ) ;
#1040 = CARTESIAN_POINT ( 'NONE',  ( 21.06408185580648862, 179.7982817377094591, -126.3732375885690260 ) ) ;
#1041 = CARTESIAN_POINT ( 'NONE',  ( -1037.461794897084019, 110.6138330393709879, -107.9061927053326144 ) ) ;
#1042 = CARTESIAN_POINT ( 'NONE',  ( 120.8820948793965186, 0.000000000000000000, -186.6989091883332890 ) ) ;
#1043 = DIRECTION ( 'NONE',  ( 0.000000000000000000, 0.000000000000000000, 1.000000000000000000 ) ) ;
#1044 = AXIS2_PLACEMENT_3D ( 'NONE', #7346, #6420, #10190 ) ;
#1045 = ORIENTED_EDGE ( 'NONE', *, *, #1101, .F. ) ;
#1046 = DIRECTION ( 'NONE',  ( 0.000000000000000000, 1.000000000000000000, -0.000000000000000000 ) ) ;
#1047 = CARTESIAN_POINT ( 'NONE',  ( -373.3860983059685168, 96.94888192596226872, -100.0157719451421201 ) ) ;
#1048 = ADVANCED_FACE ( 'NONE', ( #8799 ), #6941, .F. ) ;
#1049 = ADVANCED_FACE ( 'NONE', ( #9076 ), #5081, .F. ) ;
#1050 = ORIENTED_EDGE ( 'NONE', *, *, #6377, .F. ) ;
#1051 = CARTESIAN_POINT ( 'NONE',  ( -926.8105964072291272, 116.1567348237266515, -103.3307627799635213 ) ) ;
#1052 = CARTESIAN_POINT ( 'NONE',  ( -19.03136272649511085, 180.2041921146316668, -134.6807709998038547 ) ) ;
#1053 = CARTESIAN_POINT ( 'NONE',  ( -1045.884592419587534, 115.0579440276406871, -130.5712005305406365 ) ) ;
#1054 = CARTESIAN_POINT ( 'NONE',  ( 19.94460181908782914, 178.0949482486194597, -126.1813690857228636 ) ) ;
#1055 = CIRCLE ( 'NONE', #4008, 7.500000000000012434 ) ;
#1056 = CARTESIAN_POINT ( 'NONE',  ( -951.4198147059590838, 125.0824040815807194, -122.7172756069790864 ) ) ;
#1057 = EDGE_LOOP ( 'NONE', ( #6785, #9431, #1351, #2666, #10669 ) ) ;
#1058 = LINE ( 'NONE', #8589, #4412 ) ;
#1059 = DIRECTION ( 'NONE',  ( -0.3117078928809425831, -5.319854888938806247E-14, 0.9501779778103273122 ) ) ;
#1060 = CARTESIAN_POINT ( 'NONE',  ( -1031.000617048993718, 115.3267894020686697, -136.2353035311981557 ) ) ;
#1061 = CARTESIAN_POINT ( 'NONE',  ( -379.2435172475073841, 101.8653349591487398, -122.0127727988336233 ) ) ;
#1062 = DIRECTION ( 'NONE',  ( -8.163404592832031500E-17, 1.000000000000000000, 0.000000000000000000 ) ) ;
#1063 = CARTESIAN_POINT ( 'NONE',  ( -187.5000000000000000, -9.213203435596478030, -126.4213562373082453 ) ) ;
#1064 = ORIENTED_EDGE ( 'NONE', *, *, #2859, .T. ) ;
#1065 = DIRECTION ( 'NONE',  ( -0.000000000000000000, 1.000000000000000000, 7.930164461608263644E-17 ) ) ;
#1066 = CARTESIAN_POINT ( 'NONE',  ( -382.5082707561835491, 95.24935193720608595, -139.7187524817161659 ) ) ;
#1067 = CARTESIAN_POINT ( 'NONE',  ( -1054.691024341075263, 108.1159421897237962, -141.4553492942763739 ) ) ;
#1068 = FACE_BOUND ( 'NONE', #9922, .T. ) ;
#1069 = ORIENTED_EDGE ( 'NONE', *, *, #2927, .T. ) ;
#1070 = ORIENTED_EDGE ( 'NONE', *, *, #5111, .F. ) ;
#1071 = CARTESIAN_POINT ( 'NONE',  ( 19.96762839730446260, 179.5630691651248299, -123.3296266449212766 ) ) ;
#1072 = LINE ( 'NONE', #8442, #4255 ) ;
#1073 = DIRECTION ( 'NONE',  ( 1.000000000000000000, 8.163404592832031500E-17, 0.000000000000000000 ) ) ;
#1074 = CARTESIAN_POINT ( 'NONE',  ( -1013.637332661010191, 62.09754518945636903, -146.0307792196449839 ) ) ;
#1075 = VECTOR ( 'NONE', #9864, 1000.000000000000000 ) ;
#1076 = ORIENTED_EDGE ( 'NONE', *, *, #1114, .F. ) ;
#1077 = CARTESIAN_POINT ( 'NONE',  ( -374.3833522074543794, 72.72018747391939542, -152.7479631189390830 ) ) ;
#1078 = DIRECTION ( 'NONE',  ( -1.000000000000000000, 0.000000000000000000, 0.000000000000000000 ) ) ;
#1079 = CARTESIAN_POINT ( 'NONE',  ( -372.7333679680364753, 64.32814225526269070, -102.4919576850857936 ) ) ;
#1080 = LINE ( 'NONE', #3911, #7467 ) ;
#1081 = ORIENTED_EDGE ( 'NONE', *, *, #7850, .T. ) ;
#1082 = CARTESIAN_POINT ( 'NONE',  ( -1025.943122242211757, 53.12767954719351593, -130.5712005305404375 ) ) ;
#1083 = EDGE_CURVE ( 'NONE', #6536, #957, #334, .T. ) ;
#1084 = VECTOR ( 'NONE', #3811, 1000.000000000000000 ) ;
#1085 = EDGE_LOOP ( 'NONE', ( #10428, #11076, #8480, #3695 ) ) ;
#1086 = AXIS2_PLACEMENT_3D ( 'NONE', #9773, #2360, #1314 ) ;
#1087 = LINE ( 'NONE', #2128, #5843 ) ;
#1088 = CARTESIAN_POINT ( 'NONE',  ( -1028.007066121602975, 60.50166182213163069, -103.3307627799636350 ) ) ;
#1089 = CARTESIAN_POINT ( 'NONE',  ( 0.3563104543936067015, -6.049278984716129237, -7.522341449313000972 ) ) ;
#1090 = ORIENTED_EDGE ( 'NONE', *, *, #6921, .F. ) ;
#1091 = CARTESIAN_POINT ( 'NONE',  ( -828.0762569670757784, 76.03166466797384260, -154.6764201226847035 ) ) ;
#1092 = ORIENTED_EDGE ( 'NONE', *, *, #349, .F. ) ;
#1093 = VECTOR ( 'NONE', #5863, 1000.000000000000000 ) ;
#1094 = PRODUCT_CONTEXT ( 'NONE', #11592, 'mechanical' ) ;
#1095 = VECTOR ( 'NONE', #2198, 1000.000000000000000 ) ;
#1096 = ORIENTED_EDGE ( 'NONE', *, *, #2654, .F. ) ;
#1097 = CARTESIAN_POINT ( 'NONE',  ( -1028.454949082212806, 53.01113643315385104, -113.1262384684094400 ) ) ;
#1098 = ADVANCED_FACE ( 'NONE', ( #11061 ), #7814, .F. ) ;
#1099 = CARTESIAN_POINT ( 'NONE',  ( -119.9999999999999858, 12.00000000000001421, -126.4213562373086575 ) ) ;
#1100 = CARTESIAN_POINT ( 'NONE',  ( 35.00000000000000000, 152.0000000000000000, 190.3192290001959748 ) ) ;
#1101 = EDGE_CURVE ( 'NONE', #3987, #7340, #5116, .T. ) ;
#1102 = SHAPE_REPRESENTATION ( 'hex bolt gradeab_iso_ISO 4014 - M12 x 50 x 30-N', ( #11957 ), #5648 ) ;
#1103 = CARTESIAN_POINT ( 'NONE',  ( -974.3195816561840275, 116.7169707472884141, -107.9061927053320602 ) ) ;
#1104 = LINE ( 'NONE', #10488, #4923 ) ;
#1105 = CARTESIAN_POINT ( 'NONE',  ( -19.91567555516949994, 178.3764997479877650, -126.5185459719826468 ) ) ;
#1106 = CARTESIAN_POINT ( 'NONE',  ( 19.03136272649511085, 180.2041921146316668, -134.6807709998038547 ) ) ;
#1107 = ADVANCED_FACE ( 'NONE', ( #5426, #10197 ), #7355, .T. ) ;
#1108 = ORIENTED_EDGE ( 'NONE', *, *, #8570, .F. ) ;
#1109 = ORIENTED_EDGE ( 'NONE', *, *, #2855, .T. ) ;
#1110 = CARTESIAN_POINT ( 'NONE',  ( -1060.958858734054957, 107.4804882715807963, -107.9061927053325007 ) ) ;
#1111 =( GEOMETRIC_REPRESENTATION_CONTEXT ( 3 ) GLOBAL_UNCERTAINTY_ASSIGNED_CONTEXT ( ( #2261 ) ) GLOBAL_UNIT_ASSIGNED_CONTEXT ( ( #7770, #343, #2439 ) ) REPRESENTATION_CONTEXT ( 'NONE', 'WORKASPACE' ) );
#1112 = CARTESIAN_POINT ( 'NONE',  ( -818.8285638327247398, 78.67432280806536937, -158.6807709998041673 ) ) ;
#1113 = FACE_OUTER_BOUND ( 'NONE', #10754, .T. ) ;
#1114 = EDGE_CURVE ( 'NONE', #1499, #12174, #8297, .T. ) ;
#1115 = CARTESIAN_POINT ( 'NONE',  ( -1013.875822516560447, 120.2710389253235519, -124.6807709998039257 ) ) ;
#1116 = ORIENTED_EDGE ( 'NONE', *, *, #10704, .F. ) ;
#1117 = DIRECTION ( 'NONE',  ( 0.000000000000000000, 0.000000000000000000, -1.000000000000000000 ) ) ;
#1118 = CARTESIAN_POINT ( 'NONE',  ( -35.00000000000000000, 0.000000000000000000, 40.70327710424895429 ) ) ;
#1119 = CARTESIAN_POINT ( 'NONE',  ( -1065.000000000006366, 107.1049510380562850, -141.4553492942759192 ) ) ;
#1120 = CARTESIAN_POINT ( 'NONE',  ( -379.3756478403909682, 101.6476682939905629, -120.7185890014945784 ) ) ;
#1121 = EDGE_CURVE ( 'NONE', #818, #12110, #7480, .T. ) ;
#1122 = CARTESIAN_POINT ( 'NONE',  ( 1.249585401188644101E-12, 12.00000000000000000, -6.421356237309494119 ) ) ;
#1123 = CARTESIAN_POINT ( 'NONE',  ( -60.00000000000000000, 152.0000000000000000, -126.4213562373090696 ) ) ;
#1124 = ORIENTED_EDGE ( 'NONE', *, *, #4496, .F. ) ;
#1125 = DIRECTION ( 'NONE',  ( -1.000000000000000000, 0.000000000000000000, 0.000000000000000000 ) ) ;
#1126 = PRODUCT_DEFINITION_SHAPE ( 'NONE', 'NONE',  #406 ) ;
#1127 = CARTESIAN_POINT ( 'NONE',  ( -993.0619804577135028, 103.7129695969640579, -149.7857175106631757 ) ) ;
#1128 = DIRECTION ( 'NONE',  ( 0.000000000000000000, 0.000000000000000000, 1.000000000000000000 ) ) ;
#1129 = ORIENTED_EDGE ( 'NONE', *, *, #199, .F. ) ;
#1130 = VECTOR ( 'NONE', #12111, 1000.000000000000000 ) ;
#1131 = EDGE_CURVE ( 'NONE', #4910, #2378, #6110, .T. ) ;
#1132 = DIRECTION ( 'NONE',  ( -8.163404592832030268E-17, 1.000000000000000000, -0.000000000000000000 ) ) ;
#1133 = EDGE_LOOP ( 'NONE', ( #5075, #8034, #10647, #2735 ) ) ;
#1134 = CARTESIAN_POINT ( 'NONE',  ( 8.099999999999999645, 7.347880794884118750E-16, -5.999999999999999112 ) ) ;
#1135 = LINE ( 'NONE', #8726, #2644 ) ;
#1136 = DIRECTION ( 'NONE',  ( -1.000000000000000000, -2.040851148208007875E-17, 0.000000000000000000 ) ) ;
#1137 = CARTESIAN_POINT ( 'NONE',  ( -1062.493403002509012, 61.99900353997395541, -149.7857175106634315 ) ) ;
#1138 = ORIENTED_EDGE ( 'NONE', *, *, #11671, .T. ) ;
#1139 = CARTESIAN_POINT ( 'NONE',  ( -374.9999469826531140, 82.55142442433661643, -144.6804108797159643 ) ) ;
#1140 = CARTESIAN_POINT ( 'NONE',  ( 8.099999999999999645, 0.000000000000000000, 0.000000000000000000 ) ) ;
#1141 = ORIENTED_EDGE ( 'NONE', *, *, #8393, .T. ) ;
#1142 = CARTESIAN_POINT ( 'NONE',  ( -1032.589060384111690, 47.36392975189053800, -136.2353035311989231 ) ) ;
#1143 = EDGE_LOOP ( 'NONE', ( #4148, #428, #10091, #5318 ) ) ;
#1144 = AXIS2_PLACEMENT_3D ( 'NONE', #1240, #7036, #2348 ) ;
#1145 = CARTESIAN_POINT ( 'NONE',  ( 1.249585401188644101E-12, -6.000000000000005329, -6.421356237309495008 ) ) ;
#1146 = EDGE_CURVE ( 'NONE', #5183, #3163, #12052, .T. ) ;
#1147 = AXIS2_PLACEMENT_3D ( 'NONE', #9115, #6335, #522 ) ;
#1148 = CARTESIAN_POINT ( 'NONE',  ( -795.0000000000039790, 60.65002596136936575, -103.3307627799632797 ) ) ;
#1149 = CARTESIAN_POINT ( 'NONE',  ( -821.6103028745254733, 83.16718542005979486, -104.7144644823257522 ) ) ;
#1150 = CARTESIAN_POINT ( 'NONE',  ( -1057.693846703458348, 44.87596864925374973, -136.2353035311986957 ) ) ;
#1151 = ORIENTED_EDGE ( 'NONE', *, *, #496, .F. ) ;
#1152 = FACE_OUTER_BOUND ( 'NONE', #3781, .T. ) ;
#1153 = CARTESIAN_POINT ( 'NONE',  ( 1.874378101782966050E-12, 0.000000000000000000, 53.57864376269050410 ) ) ;
#1154 = ORIENTED_EDGE ( 'NONE', *, *, #7435, .T. ) ;
#1155 = DIRECTION ( 'NONE',  ( 0.000000000000000000, 0.000000000000000000, 1.000000000000000000 ) ) ;
#1156 = ITEM_DEFINED_TRANSFORMATION ( 'NONE', 'NONE', #7220,  #11957 ) ;
#1157 = EDGE_LOOP ( 'NONE', ( #5522, #946 ) ) ;
#1158 = CARTESIAN_POINT ( 'NONE',  ( -1063.013736978595944, 47.55218547899807646, -122.7172756069792570 ) ) ;
#1159 = STYLED_ITEM ( 'NONE', ( #3335 ), #8147 ) ;
#1160 = CARTESIAN_POINT ( 'NONE',  ( -27.99999999999999645, -492.9999999999998863, -27.99999999999999645 ) ) ;
#1161 = FACE_OUTER_BOUND ( 'NONE', #10213, .T. ) ;
#1162 = AXIS2_PLACEMENT_3D ( 'NONE', #4182, #1345, #5107 ) ;
#1163 = CARTESIAN_POINT ( 'NONE',  ( -926.5908784743340902, 123.4113341959661767, -113.1262384684093831 ) ) ;
#1164 = CYLINDRICAL_SURFACE ( 'NONE', #4575, 7.500000000000007105 ) ;
#1165 = CIRCLE ( 'NONE', #1752, 7.500000000000007105 ) ;
#1166 = EDGE_CURVE ( 'NONE', #7292, #12134, #2810, .T. ) ;
#1167 = VERTEX_POINT ( 'NONE', #6427 ) ;
#1168 = ADVANCED_FACE ( 'NONE', ( #10376 ), #7419, .F. ) ;
#1169 = SURFACE_SIDE_STYLE ('',( #10552 ) ) ;
#1170 = ORIENTED_EDGE ( 'NONE', *, *, #4570, .T. ) ;
#1171 = CARTESIAN_POINT ( 'NONE',  ( -993.6119331254994904, 96.30709745136255151, -96.78565065507915222 ) ) ;
#1172 = CIRCLE ( 'NONE', #8067, 1.500000000000001332 ) ;
#1173 = DIRECTION ( 'NONE',  ( 0.000000000000000000, 0.000000000000000000, 1.000000000000000000 ) ) ;
#1174 = VECTOR ( 'NONE', #7048, 1000.000000000000000 ) ;
#1175 = CARTESIAN_POINT ( 'NONE',  ( -974.1288507787421622, 124.2142274477005657, -122.7172756069789017 ) ) ;
#1176 = ORIENTED_EDGE ( 'NONE', *, *, #10134, .T. ) ;
#1177 = LINE ( 'NONE', #5924, #11327 ) ;
#1178 = AXIS2_PLACEMENT_3D ( 'NONE', #5862, #5742, #8485 ) ;
#1179 = DIRECTION ( 'NONE',  ( 0.000000000000000000, 1.000000000000000000, 0.000000000000000000 ) ) ;
#1180 = DIRECTION ( 'NONE',  ( 0.000000000000000000, 1.000000000000000000, 0.000000000000000000 ) ) ;
#1181 = CLOSED_SHELL ( 'NONE', ( #2542, #11758, #7956, #2235, #4789, #7074, #2002, #8291, #11705, #2213, #9575, #4708, #4730, #9794, #7659, #7989, #5207, #11669, #184, #11079, #9868, #10769, #3546, #2306, #7612, #3183, #8173, #8650, #6552, #8788, #4998, #11606, #9913, #7159, #4622, #1812, #9562, #9491, #1866, #10155, #622, #1425, #5384, #10291, #6067, #7120, #1098, #2092, #9108, #8853, #4168, #7313, #4187, #12137, #1049, #3430, #8221, #5456, #7889, #10174, #11655, #10828, #5327, #3009, #7053, #5388, #11450, #11950, #1268, #11478, #6978, #8435, #4881, #271, #4641, #10024, #8378, #2223, #6168, #5705, #5012, #492, #7320, #11734 ) ) ;
#1182 = CARTESIAN_POINT ( 'NONE',  ( -1060.958858734060186, 107.4804882715809526, -141.4553492942761750 ) ) ;
#1183 = DIRECTION ( 'NONE',  ( -0.000000000000000000, 1.000000000000000000, -0.000000000000000000 ) ) ;
#1184 = SHAPE_REPRESENTATION_RELATIONSHIP ( 'NONE' , 'NONE' ,  #4872, #6043 ) ;
#1185 = VERTEX_POINT ( 'NONE', #8357 ) ;
#1186 = CARTESIAN_POINT ( 'NONE',  ( -1054.380968608931425, 114.0683136310379524, -124.6807709998043663 ) ) ;
#1187 = EDGE_CURVE ( 'NONE', #3899, #2611, #5763, .T. ) ;
#1188 = CARTESIAN_POINT ( 'NONE',  ( -926.9570750291560444, 111.1083136274932031, -149.7857175106636021 ) ) ;
#1189 = CIRCLE ( 'NONE', #4922, 7.500000000000007105 ) ;
#1190 = AXIS2_PLACEMENT_3D ( 'NONE', #8519, #10425, #3809 ) ;
#1191 = FACE_BOUND ( 'NONE', #5209, .T. ) ;
#1192 = VERTEX_POINT ( 'NONE', #5559 ) ;
#1193 = CARTESIAN_POINT ( 'NONE',  ( -142.5000000000000000, 24.00000000000001421, -126.4213562373084301 ) ) ;
#1194 = ORIENTED_EDGE ( 'NONE', *, *, #1790, .T. ) ;
#1195 = CARTESIAN_POINT ( 'NONE',  ( -382.8391312933034669, 94.32133009973502169, -140.4452862510830755 ) ) ;
#1196 = DIRECTION ( 'NONE',  ( 0.000000000000000000, 1.000000000000000000, 0.000000000000000000 ) ) ;
#1197 = CARTESIAN_POINT ( 'NONE',  ( -975.5821371384174654, 62.83201726680850641, -152.5758913445291682 ) ) ;
#1198 = CARTESIAN_POINT ( 'NONE',  ( -384.7868575475719695, 85.94460086465754500, -144.2989652200420494 ) ) ;
#1199 = CARTESIAN_POINT ( 'NONE',  ( -151.3258811035894098, 0.000000000000000000, -63.63263083939681053 ) ) ;
#1200 = CARTESIAN_POINT ( 'NONE',  ( -374.6039973053199788, 73.23368555401432900, -106.6028248502465061 ) ) ;
#1201 = EDGE_CURVE ( 'NONE', #1440, #4090, #3564, .T. ) ;
#1202 = EDGE_LOOP ( 'NONE', ( #3605, #10463 ) ) ;
#1203 = EDGE_LOOP ( 'NONE', ( #10575, #3913, #8610, #5820 ) ) ;
#1204 = ORIENTED_EDGE ( 'NONE', *, *, #8707, .F. ) ;
#1205 = CARTESIAN_POINT ( 'NONE',  ( -902.0880155070191222, 62.23309906011806447, -107.9061927053322876 ) ) ;
#1206 = CARTESIAN_POINT ( 'NONE',  ( -19.99999999999992184, 182.7057073811386658, -124.7928861707884494 ) ) ;
#1207 = CARTESIAN_POINT ( 'NONE',  ( 30.00000000000000000, -492.9999999999998863, 30.00000000000000000 ) ) ;
#1208 = EDGE_LOOP ( 'NONE', ( #11716, #6844, #396, #5185 ) ) ;
#1209 = CARTESIAN_POINT ( 'NONE',  ( -384.5582068021247437, 87.62753060213235301, -105.4794641167554232 ) ) ;
#1210 = ORIENTED_EDGE ( 'NONE', *, *, #1523, .T. ) ;
#1211 = CARTESIAN_POINT ( 'NONE',  ( -826.8780104611989827, 74.69851342245382853, -154.6772770270139858 ) ) ;
#1212 = EDGE_LOOP ( 'NONE', ( #8401, #12199, #1064, #4026 ) ) ;
#1213 = ORIENTED_EDGE ( 'NONE', *, *, #10066, .T. ) ;
#1214 = CARTESIAN_POINT ( 'NONE',  ( -817.2011019090423360, 28.13185037056188875, -118.7903414690680250 ) ) ;
#1215 = CARTESIAN_POINT ( 'NONE',  ( 4.781971561110112670E-16, 0.4400770685300993690, -9.000000000000003553 ) ) ;
#1216 = DIRECTION ( 'NONE',  ( -1.000000000000000000, -0.000000000000000000, -0.000000000000000000 ) ) ;
#1217 = CARTESIAN_POINT ( 'NONE',  ( -1065.000000000002956, 98.77454568802522772, -99.57582448894488891 ) ) ;
#1218 = CARTESIAN_POINT ( 'NONE',  ( -19.98421530564996473, 179.1834412406901151, -125.7728037431097619 ) ) ;
#1219 = VERTEX_POINT ( 'NONE', #9205 ) ;
#1220 = PRODUCT_DEFINITION_SHAPE ( 'NONE', 'NONE',  #12245 ) ;
#1221 = CARTESIAN_POINT ( 'NONE',  ( 35.00000000000000000, 11.99999999999998046, 190.3192290001959748 ) ) ;
#1222 = VECTOR ( 'NONE', #11804, 1000.000000000000000 ) ;
#1223 = ORIENTED_EDGE ( 'NONE', *, *, #8229, .T. ) ;
#1224 = CARTESIAN_POINT ( 'NONE',  ( -974.9912860506733523, 88.33816101283738931, -95.06748246948018277 ) ) ;
#1225 = ORIENTED_EDGE ( 'NONE', *, *, #8680, .T. ) ;
#1226 = CARTESIAN_POINT ( 'NONE',  ( -951.4444194419925225, 124.5703232071644209, -130.5712005305403238 ) ) ;
#1227 = CARTESIAN_POINT ( 'NONE',  ( -1065.000000000005912, 111.6133447792291093, -130.5712005305407217 ) ) ;
#1228 = DIRECTION ( 'NONE',  ( 1.000000000000000000, 0.000000000000000000, 0.000000000000000000 ) ) ;
#1229 = EDGE_CURVE ( 'NONE', #6950, #4621, #9334, .T. ) ;
#1230 = CYLINDRICAL_SURFACE ( 'NONE', #10295, 7.500000000000007105 ) ;
#1231 = CIRCLE ( 'NONE', #8130, 7.500000000000007105 ) ;
#1232 = CARTESIAN_POINT ( 'NONE',  ( -852.8175266017512968, 121.6828083272127685, -122.7172756069790438 ) ) ;
#1233 = VERTEX_POINT ( 'NONE', #1916 ) ;
#1234 = DIRECTION ( 'NONE',  ( 0.000000000000000000, 0.000000000000000000, 1.000000000000000000 ) ) ;
#1235 = CARTESIAN_POINT ( 'NONE',  ( -819.4838385048373084, 81.17047855582150362, -104.6961160549175531 ) ) ;
#1236 = FACE_BOUND ( 'NONE', #1923, .T. ) ;
#1237 = PRESENTATION_STYLE_ASSIGNMENT (( #7913 ) ) ;
#1238 = CARTESIAN_POINT ( 'NONE',  ( -30.00000000000000000, -6.000000000000000000, 30.00000000000000000 ) ) ;
#1239 = EDGE_LOOP ( 'NONE', ( #9550, #3658, #281, #8822 ) ) ;
#1240 = CARTESIAN_POINT ( 'NONE',  ( -126.4213562373094959, -494.9999999999998863, 2.255140518769849223E-14 ) ) ;
#1241 = AXIS2_PLACEMENT_3D ( 'NONE', #6713, #7704, #3984 ) ;
#1242 = CARTESIAN_POINT ( 'NONE',  ( -954.0441199534431007, 124.9954171138389398, -126.6442663926288787 ) ) ;
#1243 = CARTESIAN_POINT ( 'NONE',  ( 144.0488662551573782, 12.00000000000000000, -146.9077238332702109 ) ) ;
#1244 = CARTESIAN_POINT ( 'NONE',  ( -853.0139081111152564, 107.1087209265616735, -146.0307792196445291 ) ) ;
#1245 = LINE ( 'NONE', #6867, #3581 ) ;
#1246 = EDGE_CURVE ( 'NONE', #11584, #8092, #6169, .T. ) ;
#1247 = ORIENTED_EDGE ( 'NONE', *, *, #5033, .F. ) ;
#1248 = ORIENTED_EDGE ( 'NONE', *, *, #3362, .F. ) ;
#1249 = AXIS2_PLACEMENT_3D ( 'NONE', #8612, #6689, #6811 ) ;
#1250 = FACE_BOUND ( 'NONE', #218, .T. ) ;
#1251 = CARTESIAN_POINT ( 'NONE',  ( -1038.283672687649414, 64.16172732404312740, -152.5758913445294240 ) ) ;
#1252 = FACE_OUTER_BOUND ( 'NONE', #4826, .T. ) ;
#1253 = DIRECTION ( 'NONE',  ( 0.000000000000000000, 0.000000000000000000, 1.000000000000000000 ) ) ;
#1254 = AXIS2_PLACEMENT_3D ( 'NONE', #6991, #1846, #12108 ) ;
#1255 = CARTESIAN_POINT ( 'NONE',  ( 126.4213562373094959, -494.9999999999998863, 7.500000000000006217 ) ) ;
#1256 = ORIENTED_EDGE ( 'NONE', *, *, #8467, .T. ) ;
#1257 = CIRCLE ( 'NONE', #2842, 7.500000000000007105 ) ;
#1258 = EDGE_CURVE ( 'NONE', #4474, #4344, #12188, .T. ) ;
#1259 = CARTESIAN_POINT ( 'NONE',  ( -954.5446161821273563, 49.54000128949434867, -118.7903414690681103 ) ) ;
#1260 = DIRECTION ( 'NONE',  ( -8.163404592832030268E-17, 1.000000000000000000, -0.000000000000000000 ) ) ;
#1261 = CARTESIAN_POINT ( 'NONE',  ( -19.99234306063619471, 182.6762740227041206, -125.2450393957101653 ) ) ;
#1262 = VERTEX_POINT ( 'NONE', #6358 ) ;
#1263 = CARTESIAN_POINT ( 'NONE',  ( -379.5535208569121437, 62.65259614875188987, -119.4499276052048771 ) ) ;
#1264 = DIRECTION ( 'NONE',  ( 0.000000000000000000, 0.000000000000000000, -1.000000000000000000 ) ) ;
#1265 = ORIENTED_EDGE ( 'NONE', *, *, #14, .F. ) ;
#1266 = CARTESIAN_POINT ( 'NONE',  ( -825.8920934164954133, 74.11705420691500024, -154.6655862438749409 ) ) ;
#1267 = ORIENTED_EDGE ( 'NONE', *, *, #1417, .T. ) ;
#1268 = ADVANCED_FACE ( 'NONE', ( #6489 ), #1795, .F. ) ;
#1269 = EDGE_CURVE ( 'NONE', #1000, #4907, #9397, .T. ) ;
#1270 = CONTEXT_DEPENDENT_SHAPE_REPRESENTATION ( #198, #3974 ) ;
#1271 = ORIENTED_EDGE ( 'NONE', *, *, #2172, .T. ) ;
#1272 = CARTESIAN_POINT ( 'NONE',  ( -795.0000000000047748, 52.00000000000024158, -122.7172756069790154 ) ) ;
#1273 = AXIS2_PLACEMENT_3D ( 'NONE', #4077, #10676, #6045 ) ;
#1274 = AXIS2_PLACEMENT_3D ( 'NONE', #10202, #9278, #11130 ) ;
#1275 = DIRECTION ( 'NONE',  ( -1.000000000000000000, 0.000000000000000000, 0.000000000000000000 ) ) ;
#1276 = UNCERTAINTY_MEASURE_WITH_UNIT (LENGTH_MEASURE( 1.000000000000000082E-05 ), #10584, 'distance_accuracy_value', 'NONE');
#1277 = ADVANCED_FACE ( 'NONE', ( #8533 ), #3766, .F. ) ;
#1278 = CARTESIAN_POINT ( 'NONE',  ( -1061.276350651669873, 98.40484402385480678, -99.57582448894525839 ) ) ;
#1279 = DIRECTION ( 'NONE',  ( -1.000000000000000000, 0.000000000000000000, 0.000000000000000000 ) ) ;
#1280 = CARTESIAN_POINT ( 'NONE',  ( 0.000000000000000000, 12.00000000000000000, -89.68077099980401101 ) ) ;
#1281 = VECTOR ( 'NONE', #4648, 1000.000000000000000 ) ;
#1282 = CIRCLE ( 'NONE', #6206, 6.599999999999998757 ) ;
#1283 = ORIENTED_EDGE ( 'NONE', *, *, #5915, .F. ) ;
#1284 = CIRCLE ( 'NONE', #89, 7.500000000000007105 ) ;
#1285 = CYLINDRICAL_SURFACE ( 'NONE', #2633, 7.500000000000007994 ) ;
#1286 = ORIENTED_EDGE ( 'NONE', *, *, #3121, .T. ) ;
#1287 = CARTESIAN_POINT ( 'NONE',  ( -1015.209561144954137, 93.46821065761379543, -95.06748246948018277 ) ) ;
#1288 = ORIENTED_EDGE ( 'NONE', *, *, #6220, .T. ) ;
#1289 = CARTESIAN_POINT ( 'NONE',  ( -823.7180591916866206, 117.1502831467254993, -130.5712005305406080 ) ) ;
#1290 = LINE ( 'NONE', #9686, #7073 ) ;
#1291 = VECTOR ( 'NONE', #5339, 1000.000000000000000 ) ;
#1292 = DIRECTION ( 'NONE',  ( -0.000000000000000000, 1.000000000000000000, 7.930164461608263644E-17 ) ) ;
#1293 = CARTESIAN_POINT ( 'NONE',  ( -852.8274699693115508, 120.9962006285026774, -118.7903414690677124 ) ) ;
#1294 = CARTESIAN_POINT ( 'NONE',  ( -305.0000000000000568, 81.99999999999995737, -89.68077099980384048 ) ) ;
#1295 = CARTESIAN_POINT ( 'NONE',  ( -67.50000000000000000, 139.9999999999999716, -126.4213562373090696 ) ) ;
#1296 = CYLINDRICAL_SURFACE ( 'NONE', #1870, 7.500000000000007105 ) ;
#1297 = DIRECTION ( 'NONE',  ( -0.000000000000000000, -1.000000000000000000, -0.000000000000000000 ) ) ;
#1298 = DIRECTION ( 'NONE',  ( 1.000000000000000000, 0.000000000000000000, 0.000000000000000000 ) ) ;
#1299 = CIRCLE ( 'NONE', #5225, 19.00000000000000000 ) ;
#1300 = DIRECTION ( 'NONE',  ( 1.000000000000000000, 0.000000000000000000, 0.000000000000000000 ) ) ;
#1301 = ORIENTED_EDGE ( 'NONE', *, *, #8271, .T. ) ;
#1302 = DIRECTION ( 'NONE',  ( 1.000000000000000000, 0.000000000000000000, -0.000000000000000000 ) ) ;
#1303 = FACE_BOUND ( 'NONE', #6936, .T. ) ;
#1304 = DIRECTION ( 'NONE',  ( 0.000000000000000000, -1.156482317317870246E-16, 1.000000000000000000 ) ) ;
#1305 = CARTESIAN_POINT ( 'NONE',  ( -1011.662592067699165, 105.4443429699074244, -149.7857175106632326 ) ) ;
#1306 = DIRECTION ( 'NONE',  ( 0.000000000000000000, 0.000000000000000000, 1.000000000000000000 ) ) ;
#1307 = LINE ( 'NONE', #6922, #12091 ) ;
#1308 = AXIS2_PLACEMENT_3D ( 'NONE', #10170, #4684, #5533 ) ;
#1309 = EDGE_LOOP ( 'NONE', ( #11192, #9487, #5444, #2692 ) ) ;
#1310 = CARTESIAN_POINT ( 'NONE',  ( 19.97422267005788044, 181.0592659262004247, -123.4551364493781733 ) ) ;
#1311 = CARTESIAN_POINT ( 'NONE',  ( -823.4970567115327640, 73.67398878492954850, -106.4962298347511620 ) ) ;
#1312 = EDGE_CURVE ( 'NONE', #4553, #11886, #371, .T. ) ;
#1313 = DIRECTION ( 'NONE',  ( 2.040851148208007875E-17, -1.000000000000000000, -0.000000000000000000 ) ) ;
#1314 = DIRECTION ( 'NONE',  ( 0.000000000000000000, 0.000000000000000000, 1.000000000000000000 ) ) ;
#1315 = CARTESIAN_POINT ( 'NONE',  ( -820.0645691041015652, 75.36693519558788523, -94.68454641646253833 ) ) ;
#1316 = EDGE_CURVE ( 'NONE', #9732, #7035, #847, .T. ) ;
#1317 = AXIS2_PLACEMENT_3D ( 'NONE', #7563, #10403, #1944 ) ;
#1318 = ORIENTED_EDGE ( 'NONE', *, *, #10928, .F. ) ;
#1319 = EDGE_CURVE ( 'NONE', #6750, #5569, #8539, .T. ) ;
#1320 = CARTESIAN_POINT ( 'NONE',  ( -854.0393178910176175, 26.93106345811105840, -113.1262384684097100 ) ) ;
#1321 = DIRECTION ( 'NONE',  ( 0.000000000000000000, 1.224646799147353207E-16, 1.000000000000000000 ) ) ;
#1322 = CARTESIAN_POINT ( 'NONE',  ( -19.85981914806637860, 181.2821069731401735, -127.0472120087121652 ) ) ;
#1323 = FACE_OUTER_BOUND ( 'NONE', #10059, .T. ) ;
#1324 = CIRCLE ( 'NONE', #7436, 7.500000000000007105 ) ;
#1325 = FACE_OUTER_BOUND ( 'NONE', #1959, .T. ) ;
#1326 = CARTESIAN_POINT ( 'NONE',  ( 6.899999999999999467, -5.196152422706638241, -9.000000000000001776 ) ) ;
#1327 = ORIENTED_EDGE ( 'NONE', *, *, #2177, .F. ) ;
#1328 = CARTESIAN_POINT ( 'NONE',  ( 4.808665244885994618E-14, 0.000000000000000000, 141.4213562373094817 ) ) ;
#1329 = VERTEX_POINT ( 'NONE', #10442 ) ;
#1330 = VERTEX_POINT ( 'NONE', #9693 ) ;
#1331 = CARTESIAN_POINT ( 'NONE',  ( -954.4431216459856842, 51.77564274757639140, -113.1262384684095537 ) ) ;
#1332 = EDGE_CURVE ( 'NONE', #4924, #2829, #4976, .T. ) ;
#1333 = AXIS2_PLACEMENT_3D ( 'NONE', #6232, #6112, #9997 ) ;
#1334 = DIRECTION ( 'NONE',  ( 0.000000000000000000, 0.000000000000000000, -1.000000000000000000 ) ) ;
#1335 = AXIS2_PLACEMENT_3D ( 'NONE', #4486, #3599, #5334 ) ;
#1336 = VECTOR ( 'NONE', #3342, 1000.000000000000000 ) ;
#1337 = CARTESIAN_POINT ( 'NONE',  ( -954.5323978148114747, 113.6695689568732206, -103.3307627799632513 ) ) ;
#1338 = DIRECTION ( 'NONE',  ( -1.000000000000000000, -1.486905836551548832E-16, 0.000000000000000000 ) ) ;
#1339 = ORIENTED_EDGE ( 'NONE', *, *, #10551, .F. ) ;
#1340 = CARTESIAN_POINT ( 'NONE',  ( 1.249585401188644101E-12, -6.000000000000005329, -6.421356237309495008 ) ) ;
#1341 = COLOUR_RGB ( '', 0.08235294, 0.09019608, 0.10196078) ;
#1342 = VERTEX_POINT ( 'NONE', #7847 ) ;
#1343 = CARTESIAN_POINT ( 'NONE',  ( -1025.928429817214464, 97.79385104913474436, -96.78565065507955012 ) ) ;
#1344 = EDGE_CURVE ( 'NONE', #233, #4125, #7080, .T. ) ;
#1345 = DIRECTION ( 'NONE',  ( 0.3117078928809249860, 1.670400663243698742E-14, -0.9501779778103330854 ) ) ;
#1346 = CARTESIAN_POINT ( 'NONE',  ( -823.7697810748826441, 117.7733807739869292, -126.6442663926291914 ) ) ;
#1347 = PLANE ( 'NONE',  #12013 ) ;
#1348 = CARTESIAN_POINT ( 'NONE',  ( 19.94418390071693281, 178.3880804771991677, -123.1813497959713004 ) ) ;
#1349 =( GEOMETRIC_REPRESENTATION_CONTEXT ( 3 ) GLOBAL_UNCERTAINTY_ASSIGNED_CONTEXT ( ( #11660 ) ) GLOBAL_UNIT_ASSIGNED_CONTEXT ( ( #752, #8169, #4338 ) ) REPRESENTATION_CONTEXT ( 'NONE', 'WORKASPACE' ) );
#1350 = CARTESIAN_POINT ( 'NONE',  ( -1037.392967692957200, 114.2240391150264855, -113.1262384684098805 ) ) ;
#1351 = ORIENTED_EDGE ( 'NONE', *, *, #11667, .T. ) ;
#1352 = CARTESIAN_POINT ( 'NONE',  ( -826.0484035456422589, 83.16661265238070655, -104.7144245788473000 ) ) ;
#1353 = CARTESIAN_POINT ( 'NONE',  ( -854.0902776497798641, 23.28889115110666808, -124.6807709998044800 ) ) ;
#1354 = CARTESIAN_POINT ( 'NONE',  ( -373.2899463707186669, 98.65819193945954169, -113.5174344538613411 ) ) ;
#1355 = CARTESIAN_POINT ( 'NONE',  ( 21.06813109674855156, 179.2925129078113571, -126.1227452162743674 ) ) ;
#1356 = VECTOR ( 'NONE', #973, 1000.000000000000000 ) ;
#1357 = ORIENTED_EDGE ( 'NONE', *, *, #9119, .T. ) ;
#1358 = DIRECTION ( 'NONE',  ( -8.163404592832030268E-17, 1.000000000000000000, -0.000000000000000000 ) ) ;
#1359 = CARTESIAN_POINT ( 'NONE',  ( -1065.000000000006594, 112.0000000000007105, -124.6807709998041531 ) ) ;
#1360 = AXIS2_PLACEMENT_3D ( 'NONE', #7115, #7050, #5314 ) ;
#1361 = DIRECTION ( 'NONE',  ( -0.000000000000000000, 1.000000000000000000, -0.000000000000000000 ) ) ;
#1362 = CARTESIAN_POINT ( 'NONE',  ( -374.6494996980943597, 74.87479940665586753, -95.76181135420617352 ) ) ;
#1363 = CARTESIAN_POINT ( 'NONE',  ( 35.00000000000000000, 81.99999999999998579, 190.3192290001959748 ) ) ;
#1364 = CIRCLE ( 'NONE', #11242, 7.500000000000020428 ) ;
#1365 = EDGE_LOOP ( 'NONE', ( #487, #8976, #6117 ) ) ;
#1366 = CARTESIAN_POINT ( 'NONE',  ( -383.3184125885782692, 71.07417258413192940, -141.4727867585951344 ) ) ;
#1367 = CARTESIAN_POINT ( 'NONE',  ( -1019.723937646960849, 86.79129919622100431, -154.8742214401232502 ) ) ;
#1368 = CARTESIAN_POINT ( 'NONE',  ( -217.5000000000000000, 24.00000000000000711, -126.4213562373080180 ) ) ;
#1369 = CARTESIAN_POINT ( 'NONE',  ( 4.285787411236815022E-15, 24.00000000000001776, -126.4213562373094959 ) ) ;
#1370 = CARTESIAN_POINT ( 'NONE',  ( -822.5396358769451126, 73.84052889928489094, -94.71353457946125332 ) ) ;
#1371 = CARTESIAN_POINT ( 'NONE',  ( -210.0000000000000000, -9.213203435596478030, -126.4213562373080180 ) ) ;
#1372 = CIRCLE ( 'NONE', #166, 7.500000000000012434 ) ;
#1373 = AXIS2_PLACEMENT_3D ( 'NONE', #6165, #1466, #352 ) ;
#1374 = VERTEX_POINT ( 'NONE', #6856 ) ;
#1375 = CARTESIAN_POINT ( 'NONE',  ( -1038.401083800579045, 57.54275223462362021, -149.7857175106632326 ) ) ;
#1376 = ORIENTED_EDGE ( 'NONE', *, *, #3295, .T. ) ;
#1377 = ADVANCED_FACE ( 'NONE', ( #9751 ), #1296, .F. ) ;
#1378 = CARTESIAN_POINT ( 'NONE',  ( 20.91518010789754456, 178.8209456716285501, -124.2613132543053638 ) ) ;
#1379 = CARTESIAN_POINT ( 'NONE',  ( -976.2517683711888594, 35.25052392388814582, -122.7172756069790296 ) ) ;
#1380 = DIRECTION ( 'NONE',  ( -1.000000000000000000, 0.000000000000000000, 0.000000000000000000 ) ) ;
#1381 = ORIENTED_EDGE ( 'NONE', *, *, #2835, .T. ) ;
#1382 = DIRECTION ( 'NONE',  ( -0.000000000000000000, -1.000000000000000000, -0.000000000000000000 ) ) ;
#1383 = ORIENTED_EDGE ( 'NONE', *, *, #9854, .F. ) ;
#1384 = ORIENTED_EDGE ( 'NONE', *, *, #7764, .F. ) ;
#1385 = ORIENTED_EDGE ( 'NONE', *, *, #6553, .F. ) ;
#1386 = CARTESIAN_POINT ( 'NONE',  ( 0.000000000000000000, 0.000000000000000000, -89.68077099980401101 ) ) ;
#1387 = UNCERTAINTY_MEASURE_WITH_UNIT (LENGTH_MEASURE( 1.000000000000000082E-05 ), #8332, 'distance_accuracy_value', 'NONE');
#1388 = ADVANCED_FACE ( 'NONE', ( #3889 ), #291, .F. ) ;
#1389 = CARTESIAN_POINT ( 'NONE',  ( 87.04832655144112152, 0.000000000000000000, -210.4289243767383368 ) ) ;
#1390 = EDGE_CURVE ( 'NONE', #7340, #3987, #8949, .T. ) ;
#1391 = CARTESIAN_POINT ( 'NONE',  ( -1065.000000000004093, 93.55451860843899681, -96.78565065507908116 ) ) ;
#1392 = DIRECTION ( 'NONE',  ( -0.000000000000000000, -1.000000000000000000, -0.000000000000000000 ) ) ;
#1393 = ORIENTED_EDGE ( 'NONE', *, *, #4461, .F. ) ;
#1394 = CYLINDRICAL_SURFACE ( 'NONE', #8761, 7.500000000000007105 ) ;
#1395 = CARTESIAN_POINT ( 'NONE',  ( -370.4431240880616656, 57.15653990293294839, -114.9924028573224035 ) ) ;
#1396 = VERTEX_POINT ( 'NONE', #9514 ) ;
#1397 = LINE ( 'NONE', #4245, #462 ) ;
#1398 = ORIENTED_EDGE ( 'NONE', *, *, #12116, .F. ) ;
#1399 = CARTESIAN_POINT ( 'NONE',  ( -820.0633694947518961, 81.98028010177233682, -154.3548397009152779 ) ) ;
#1400 = CARTESIAN_POINT ( 'NONE',  ( -1037.899050076301137, 86.18944477603540122, -95.06748246948046699 ) ) ;
#1401 = CYLINDRICAL_SURFACE ( 'NONE', #1751, 7.500000000000007105 ) ;
#1402 = CARTESIAN_POINT ( 'NONE',  ( -904.1919162299276422, 124.8346192645298487, -130.5712005305403807 ) ) ;
#1403 = CARTESIAN_POINT ( 'NONE',  ( -1030.931480980267906, 117.9615145441170654, -124.6807709998043521 ) ) ;
#1404 = DIRECTION ( 'NONE',  ( -1.000000000000000000, -0.000000000000000000, 0.000000000000000000 ) ) ;
#1405 = CIRCLE ( 'NONE', #2989, 7.500000000000007105 ) ;
#1406 = CARTESIAN_POINT ( 'NONE',  ( 28.53314250459842327, 180.2041921146317236, -137.7978499286132319 ) ) ;
#1407 = EDGE_CURVE ( 'NONE', #11206, #8134, #1058, .T. ) ;
#1408 = ADVANCED_FACE ( 'NONE', ( #7660 ), #11430, .F. ) ;
#1409 = FACE_BOUND ( 'NONE', #5480, .T. ) ;
#1410 = DIRECTION ( 'NONE',  ( 0.000000000000000000, 0.000000000000000000, 1.000000000000000000 ) ) ;
#1411 = CIRCLE ( 'NONE', #8337, 7.500000000000007105 ) ;
#1412 = CARTESIAN_POINT ( 'NONE',  ( 20.71964524312697620, 180.0370539397483185, -123.3053720114571519 ) ) ;
#1413 = DIRECTION ( 'NONE',  ( -1.000000000000000000, 0.000000000000000000, 0.000000000000000000 ) ) ;
#1414 = VERTEX_POINT ( 'NONE', #5983 ) ;
#1415 = DIRECTION ( 'NONE',  ( 0.000000000000000000, 1.000000000000000000, 0.000000000000000000 ) ) ;
#1416 = CARTESIAN_POINT ( 'NONE',  ( -852.8175266017517515, 121.6828083272129106, -126.6442663926292624 ) ) ;
#1417 = EDGE_CURVE ( 'NONE', #1330, #4052, #621, .T. ) ;
#1418 = EDGE_CURVE ( 'NONE', #8166, #12110, #10504, .T. ) ;
#1419 = CARTESIAN_POINT ( 'NONE',  ( -19.03136272649511085, 180.2041921146316668, -134.6807709998038547 ) ) ;
#1420 = CARTESIAN_POINT ( 'NONE',  ( -202.4999999999999716, 151.9999999999999716, -126.4213562373080180 ) ) ;
#1421 = CARTESIAN_POINT ( 'NONE',  ( -374.0142209343122772, 70.27728921848439825, -97.82681790556920021 ) ) ;
#1422 = DIRECTION ( 'NONE',  ( 0.000000000000000000, 0.000000000000000000, 1.000000000000000000 ) ) ;
#1423 = ORIENTED_EDGE ( 'NONE', *, *, #948, .F. ) ;
#1424 = ORIENTED_EDGE ( 'NONE', *, *, #8431, .F. ) ;
#1425 = ADVANCED_FACE ( 'NONE', ( #9933, #4261, #1468, #6971, #3253, #2278, #1409, #10985, #5227, #4373, #4315, #404, #6046, #3368, #533, #7031, #8089, #8027, #11796, #9814, #8144, #8999, #2511, #7155, #10801, #10922 ), #2453, .T. ) ;
#1426 = VECTOR ( 'NONE', #7389, 1000.000000000000000 ) ;
#1427 = CARTESIAN_POINT ( 'NONE',  ( -379.7840584701665421, 63.05619850801249981, -131.1209148564447275 ) ) ;
#1428 = DIRECTION ( 'NONE',  ( -1.000000000000000000, 0.000000000000000000, 0.000000000000000000 ) ) ;
#1429 = LINE ( 'NONE', #6874, #9250 ) ;
#1430 = DIRECTION ( 'NONE',  ( -1.000000000000000000, 0.000000000000000000, 0.000000000000000000 ) ) ;
#1431 = CARTESIAN_POINT ( 'NONE',  ( -6.106226635438360972E-13, 12.00000000000000000, -244.6807709998039400 ) ) ;
#1432 = VECTOR ( 'NONE', #8423, 1000.000000000000000 ) ;
#1433 = ORIENTED_EDGE ( 'NONE', *, *, #11520, .T. ) ;
#1434 = CARTESIAN_POINT ( 'NONE',  ( -954.0832773815118344, 60.15510303592687080, -146.0307792196447565 ) ) ;
#1435 = AXIS2_PLACEMENT_3D ( 'NONE', #5645, #4409, #4607 ) ;
#1436 = ORIENTED_EDGE ( 'NONE', *, *, #10649, .T. ) ;
#1437 = CARTESIAN_POINT ( 'NONE',  ( -998.0431609429222135, 37.14019503514177956, -122.7172756069792854 ) ) ;
#1438 = ORIENTED_EDGE ( 'NONE', *, *, #5723, .F. ) ;
#1439 = DIRECTION ( 'NONE',  ( -1.000000000000000000, 0.000000000000000000, 0.000000000000000000 ) ) ;
#1440 = VERTEX_POINT ( 'NONE', #2340 ) ;
#1441 = CARTESIAN_POINT ( 'NONE',  ( -67.49999999999998579, 12.00000000000001421, -126.4213562373090696 ) ) ;
#1442 = CIRCLE ( 'NONE', #9353, 7.500000000000007105 ) ;
#1443 = DIRECTION ( 'NONE',  ( 1.000000000000000000, 0.000000000000000000, 0.000000000000000000 ) ) ;
#1444 = CARTESIAN_POINT ( 'NONE',  ( -1054.913455627178109, 103.6024512377076263, -103.3307627799635640 ) ) ;
#1445 = CARTESIAN_POINT ( 'NONE',  ( 141.4213562373095101, -6.000000000000000000, -1.508194112741312283E-14 ) ) ;
#1446 = CARTESIAN_POINT ( 'NONE',  ( 144.0488662551573782, 12.00000000000000000, -154.4077238332702393 ) ) ;
#1447 = ORIENTED_EDGE ( 'NONE', *, *, #5229, .T. ) ;
#1448 = FACE_OUTER_BOUND ( 'NONE', #11473, .T. ) ;
#1449 = CARTESIAN_POINT ( 'NONE',  ( -372.7937968025706255, 63.34872752675727270, -117.4098597798456041 ) ) ;
#1450 = VECTOR ( 'NONE', #6580, 1000.000000000000000 ) ;
#1451 = CARTESIAN_POINT ( 'NONE',  ( -270.0000000000000000, 151.9999999999999716, -126.4213562373076059 ) ) ;
#1452 = EDGE_CURVE ( 'NONE', #8333, #2076, #1529, .T. ) ;
#1453 = CIRCLE ( 'NONE', #4229, 1.500000000000001332 ) ;
#1454 = CARTESIAN_POINT ( 'NONE',  ( 126.4213562373094959, 12.00000000000000000, -7.500000000000020428 ) ) ;
#1455 = VERTEX_POINT ( 'NONE', #8934 ) ;
#1456 = FACE_OUTER_BOUND ( 'NONE', #5053, .T. ) ;
#1457 = EDGE_CURVE ( 'NONE', #3163, #7119, #2798, .T. ) ;
#1458 = CARTESIAN_POINT ( 'NONE',  ( 1.387778780781445676E-14, 152.0000000000000284, 133.9213562373095101 ) ) ;
#1459 = CARTESIAN_POINT ( 'NONE',  ( -955.0000000000038654, 102.0000000000005400, -124.6807709998041531 ) ) ;
#1460 = CARTESIAN_POINT ( 'NONE',  ( -828.8285638327243987, 78.67432280806596623, -144.4023295390031194 ) ) ;
#1461 = VECTOR ( 'NONE', #6301, 1000.000000000000000 ) ;
#1462 = EDGE_CURVE ( 'NONE', #11305, #5102, #6287, .T. ) ;
#1463 = VECTOR ( 'NONE', #10507, 1000.000000000000000 ) ;
#1464 = AXIS2_PLACEMENT_3D ( 'NONE', #6953, #10721, #7642 ) ;
#1465 = CARTESIAN_POINT ( 'NONE',  ( -823.7180591916842332, 117.1502831467252150, -118.7903414690680535 ) ) ;
#1466 = DIRECTION ( 'NONE',  ( 0.000000000000000000, 1.000000000000000000, -0.000000000000000000 ) ) ;
#1467 = CARTESIAN_POINT ( 'NONE',  ( -305.0000000000000568, 151.9999999999999716, -159.6807709998038547 ) ) ;
#1468 = FACE_BOUND ( 'NONE', #7001, .T. ) ;
#1469 = LINE ( 'NONE', #4374, #2539 ) ;
#1470 = LINE ( 'NONE', #4375, #276 ) ;
#1471 =( REPRESENTATION_RELATIONSHIP ('NONE','NONE', #12149, #1102 ) REPRESENTATION_RELATIONSHIP_WITH_TRANSFORMATION ( #8414 )SHAPE_REPRESENTATION_RELATIONSHIP( ) );
#1472 = CARTESIAN_POINT ( 'NONE',  ( -822.5268906875147650, 83.51316246527650833, -95.22287600579254274 ) ) ;
#1473 = FACE_OUTER_BOUND ( 'NONE', #8723, .T. ) ;
#1474 = CARTESIAN_POINT ( 'NONE',  ( -1017.810720698609543, 119.7719591276204625, -124.6807709998040679 ) ) ;
#1475 = AXIS2_PLACEMENT_3D ( 'NONE', #65, #3902, #8672 ) ;
#1476 = AXIS2_PLACEMENT_3D ( 'NONE', #10075, #7237, #11202 ) ;
#1477 = LINE ( 'NONE', #11189, #6951 ) ;
#1478 = DIRECTION ( 'NONE',  ( -8.163404592832030268E-17, 1.000000000000000000, -0.000000000000000000 ) ) ;
#1479 = CARTESIAN_POINT ( 'NONE',  ( -373.6864081855313202, 68.44581660449321703, -98.94085437915049397 ) ) ;
#1480 = EDGE_CURVE ( 'NONE', #6424, #6402, #662, .T. ) ;
#1481 = DIRECTION ( 'NONE',  ( 0.000000000000000000, -1.000000000000000000, 0.000000000000000000 ) ) ;
#1482 = EDGE_LOOP ( 'NONE', ( #2546, #3392, #12236, #9462 ) ) ;
#1483 = ORIENTED_EDGE ( 'NONE', *, *, #2370, .F. ) ;
#1484 = PRODUCT_RELATED_PRODUCT_CATEGORY ( 'part', '', ( #10588 ) ) ;
#1485 = AXIS2_PLACEMENT_3D ( 'NONE', #575, #1758, #3529 ) ;
#1486 = VECTOR ( 'NONE', #10909, 1000.000000000000000 ) ;
#1487 = CARTESIAN_POINT ( 'NONE',  ( 0.000000000000000000, -58.00000000000000711, -118.9213562373094817 ) ) ;
#1488 = CARTESIAN_POINT ( 'NONE',  ( -794.9999999999992042, 76.10956187831466480, -154.2940595301278393 ) ) ;
#1489 = CYLINDRICAL_SURFACE ( 'NONE', #11185, 7.500000000000007105 ) ;
#1490 = DIRECTION ( 'NONE',  ( 0.000000000000000000, 1.000000000000000000, 0.000000000000000000 ) ) ;
#1491 = CARTESIAN_POINT ( 'NONE',  ( 0.000000000000000000, 152.0000000000000000, -89.68077099980384048 ) ) ;
#1492 = CYLINDRICAL_SURFACE ( 'NONE', #11425, 35.00000000000000000 ) ;
#1493 = VERTEX_POINT ( 'NONE', #7121 ) ;
#1494 = CARTESIAN_POINT ( 'NONE',  ( -1065.000000000000909, 56.89504896194504369, -141.4553492942757771 ) ) ;
#1495 = EDGE_CURVE ( 'NONE', #2379, #1167, #5320, .T. ) ;
#1496 = EDGE_LOOP ( 'NONE', ( #3127, #7189 ) ) ;
#1497 = EDGE_LOOP ( 'NONE', ( #11987, #7229, #521, #8305 ) ) ;
#1498 = FACE_OUTER_BOUND ( 'NONE', #3824, .T. ) ;
#1499 = VERTEX_POINT ( 'NONE', #11826 ) ;
#1500 = CARTESIAN_POINT ( 'NONE',  ( 1.387778780781445676E-14, -492.9999999999998863, 126.4213562373094959 ) ) ;
#1501 = CARTESIAN_POINT ( 'NONE',  ( -373.7456202422138176, 96.52126932011218230, -138.5319469839025714 ) ) ;
#1502 = FACE_OUTER_BOUND ( 'NONE', #6460, .T. ) ;
#1503 = ORIENTED_EDGE ( 'NONE', *, *, #12036, .F. ) ;
#1504 = AXIS2_PLACEMENT_3D ( 'NONE', #5650, #9422, #8504 ) ;
#1505 = ORIENTED_EDGE ( 'NONE', *, *, #349, .T. ) ;
#1506 = CARTESIAN_POINT ( 'NONE',  ( -151.3258811035894098, 12.00000000000000000, -63.63263083939681053 ) ) ;
#1507 = FACE_OUTER_BOUND ( 'NONE', #10961, .T. ) ;
#1508 = AXIS2_PLACEMENT_3D ( 'NONE', #4557, #2694, #9310 ) ;
#1509 = CARTESIAN_POINT ( 'NONE',  ( -903.2629211055218548, 97.63080833215146015, -95.06748246947979908 ) ) ;
#1510 = DIRECTION ( 'NONE',  ( 0.000000000000000000, 0.000000000000000000, 1.000000000000000000 ) ) ;
#1511 = ORIENTED_EDGE ( 'NONE', *, *, #12140, .F. ) ;
#1512 = CARTESIAN_POINT ( 'NONE',  ( -150.0000000000000000, 24.00000000000001421, -126.4213562373084301 ) ) ;
#1513 = ORIENTED_EDGE ( 'NONE', *, *, #6743, .T. ) ;
#1514 = CARTESIAN_POINT ( 'NONE',  ( 0.000000000000000000, -492.9999999999998863, 0.000000000000000000 ) ) ;
#1515 = DIRECTION ( 'NONE',  ( -1.000000000000000000, 0.000000000000000000, 0.000000000000000000 ) ) ;
#1516 = ORIENTED_EDGE ( 'NONE', *, *, #5402, .F. ) ;
#1517 = CARTESIAN_POINT ( 'NONE',  ( -35.00000000000000000, 12.00000000000001954, -124.6807709998040110 ) ) ;
#1518 = CARTESIAN_POINT ( 'NONE',  ( -1019.723937646958007, 86.79129919622097589, -94.48732055948626396 ) ) ;
#1519 = CIRCLE ( 'NONE', #9424, 35.00000000000000000 ) ;
#1520 = CARTESIAN_POINT ( 'NONE',  ( 19.90865200055593220, 181.4799304009739558, -122.7714319726113104 ) ) ;
#1521 = CARTESIAN_POINT ( 'NONE',  ( -954.0441199534440102, 124.9954171138387977, -124.6807709998039115 ) ) ;
#1522 = DIRECTION ( 'NONE',  ( -0.000000000000000000, 1.000000000000000000, 7.930164461608263644E-17 ) ) ;
#1523 = EDGE_CURVE ( 'NONE', #2536, #6732, #761, .T. ) ;
#1524 = DIRECTION ( 'NONE',  ( -8.163404592832030268E-17, 1.000000000000000000, -0.000000000000000000 ) ) ;
#1525 = AXIS2_PLACEMENT_3D ( 'NONE', #4084, #10684, #7854 ) ;
#1526 = CARTESIAN_POINT ( 'NONE',  ( -820.7495229154725394, 74.72132575352334527, -143.3103177350645296 ) ) ;
#1527 = ADVANCED_FACE ( 'NONE', ( #1753 ), #6197, .F. ) ;
#1528 = CONICAL_SURFACE ( 'NONE', #7858, 9.000000000000000000, 1.047197551196600296 ) ;
#1529 = LINE ( 'NONE', #5287, #5068 ) ;
#1530 = LINE ( 'NONE', #11678, #9648 ) ;
#1531 = DIRECTION ( 'NONE',  ( -3.061276722312011504E-17, 1.000000000000000000, -0.000000000000000000 ) ) ;
#1532 = ORIENTED_EDGE ( 'NONE', *, *, #10312, .T. ) ;
#1533 = CARTESIAN_POINT ( 'NONE',  ( 4.255174644013695128E-15, 25.00000000000002132, -126.4213562373094959 ) ) ;
#1534 = CARTESIAN_POINT ( 'NONE',  ( -926.5138833012647410, 125.7648744980332225, -124.6807709998040394 ) ) ;
#1535 = DIRECTION ( 'NONE',  ( -1.000000000000000000, 0.000000000000000000, 0.000000000000000000 ) ) ;
#1536 = DIRECTION ( 'NONE',  ( 0.000000000000000000, -1.156482317317870246E-16, 1.000000000000000000 ) ) ;
#1537 = CARTESIAN_POINT ( 'NONE',  ( -370.5981920676458685, 57.56502298018414621, -113.6242979122189922 ) ) ;
#1538 = CIRCLE ( 'NONE', #12208, 7.500000000000007105 ) ;
#1539 = CYLINDRICAL_SURFACE ( 'NONE', #8352, 7.500000000000007105 ) ;
#1540 = ORIENTED_EDGE ( 'NONE', *, *, #9548, .T. ) ;
#1541 = ADVANCED_FACE ( 'NONE', ( #1498 ), #4158, .F. ) ;
#1542 = CARTESIAN_POINT ( 'NONE',  ( -19.98431733801637122, 177.9165942756023640, -123.8639317673912785 ) ) ;
#1543 = DIRECTION ( 'NONE',  ( 1.000000000000000000, 1.186840563529527301E-16, 0.000000000000000000 ) ) ;
#1544 = VECTOR ( 'NONE', #7610, 1000.000000000000000 ) ;
#1545 = EDGE_CURVE ( 'NONE', #8717, #4751, #224, .T. ) ;
#1546 = DIRECTION ( 'NONE',  ( -0.000000000000000000, 1.000000000000000000, 0.000000000000000000 ) ) ;
#1547 = CARTESIAN_POINT ( 'NONE',  ( -363.0000000000000568, 81.99999999999995737, -89.68077099980384048 ) ) ;
#1548 = DIRECTION ( 'NONE',  ( -0.000000000000000000, 1.000000000000000000, -0.000000000000000000 ) ) ;
#1549 = CARTESIAN_POINT ( 'NONE',  ( -828.8285638327240576, 78.67432280806576728, -94.77914401073080342 ) ) ;
#1550 = DIRECTION ( 'NONE',  ( -1.000000000000000000, 0.000000000000000000, 0.000000000000000000 ) ) ;
#1551 = ORIENTED_EDGE ( 'NONE', *, *, #2991, .T. ) ;
#1552 = CARTESIAN_POINT ( 'NONE',  ( -1038.595419435783924, 46.89684673038589580, -141.4553492942758623 ) ) ;
#1553 = VECTOR ( 'NONE', #3704, 1000.000000000000000 ) ;
#1554 = ORIENTED_EDGE ( 'NONE', *, *, #9478, .T. ) ;
#1555 = CARTESIAN_POINT ( 'NONE',  ( -19.97950307607502296, 180.8737719992032567, -126.0168746971561688 ) ) ;
#1556 = DIRECTION ( 'NONE',  ( -0.000000000000000000, -1.000000000000000000, -1.757987137413040192E-14 ) ) ;
#1557 = CARTESIAN_POINT ( 'NONE',  ( 4.808665244885994618E-14, -494.9999999999998863, 141.4213562373094817 ) ) ;
#1558 = EDGE_CURVE ( 'NONE', #11124, #5668, #5379, .T. ) ;
#1559 = ORIENTED_EDGE ( 'NONE', *, *, #7371, .T. ) ;
#1560 = EDGE_CURVE ( 'NONE', #9452, #495, #3946, .T. ) ;
#1561 = CARTESIAN_POINT ( 'NONE',  ( -380.7611941007019141, 64.86892148911482536, -135.0070643092065836 ) ) ;
#1562 = CARTESIAN_POINT ( 'NONE',  ( -381.5042408296175722, 97.59833250969687413, -112.1498553144568717 ) ) ;
#1563 = AXIS2_PLACEMENT_3D ( 'NONE', #10918, #10856, #11737 ) ;
#1564 = ORIENTED_EDGE ( 'NONE', *, *, #5371, .T. ) ;
#1565 = DIRECTION ( 'NONE',  ( 0.000000000000000000, 0.000000000000000000, 1.000000000000000000 ) ) ;
#1566 = ORIENTED_EDGE ( 'NONE', *, *, #7764, .T. ) ;
#1567 = CARTESIAN_POINT ( 'NONE',  ( -928.4368846968637854, 59.55532739646334051, -126.6442663926292056 ) ) ;
#1568 = CARTESIAN_POINT ( 'NONE',  ( -180.0000000000000000, -9.213203435596478030, -126.4213562373082453 ) ) ;
#1569 = AXIS2_PLACEMENT_3D ( 'NONE', #11542, #273, #10607 ) ;
#1570 = CARTESIAN_POINT ( 'NONE',  ( 0.8038475772933606489, 5.196152422706624918, 8.999999999999998224 ) ) ;
#1571 = CARTESIAN_POINT ( 'NONE',  ( -819.4913475613807350, 81.18356759358016461, -154.4422483361309446 ) ) ;
#1572 = CARTESIAN_POINT ( 'NONE',  ( -1047.151245865161172, 77.61790247226321071, -94.48732055948626396 ) ) ;
#1573 = CARTESIAN_POINT ( 'NONE',  ( 7.500000000000020428, 12.00000000000001776, -126.4213562373094959 ) ) ;
#1574 = CARTESIAN_POINT ( 'NONE',  ( -7.500000000000007105, 139.9999999999999716, -126.4213562373094959 ) ) ;
#1575 = CARTESIAN_POINT ( 'NONE',  ( -385.0247828397638159, 81.99275599918267687, -104.6365852498861102 ) ) ;
#1576 = EDGE_LOOP ( 'NONE', ( #4875, #298 ) ) ;
#1577 = CARTESIAN_POINT ( 'NONE',  ( 4.285787411236815022E-15, 24.00000000000001776, -126.4213562373094959 ) ) ;
#1578 = LINE ( 'NONE', #1706, #1486 ) ;
#1579 = ORIENTED_EDGE ( 'NONE', *, *, #2760, .T. ) ;
#1580 = DIRECTION ( 'NONE',  ( -1.000000000000000000, 0.000000000000000000, 0.000000000000000000 ) ) ;
#1581 = CARTESIAN_POINT ( 'NONE',  ( -927.4753839990671622, 92.66010094724835255, -94.48732055948569553 ) ) ;
#1582 = CARTESIAN_POINT ( 'NONE',  ( 0.5590800469813623774, 9.968355046870078340, 0.7343025909353934066 ) ) ;
#1583 = CARTESIAN_POINT ( 'NONE',  ( -6.106226635438360972E-13, 0.000000000000000000, -252.1807709998039115 ) ) ;
#1584 = DIRECTION ( 'NONE',  ( -0.000000000000000000, -0.000000000000000000, 1.000000000000000000 ) ) ;
#1585 = DIRECTION ( 'NONE',  ( 0.000000000000000000, 0.000000000000000000, 1.000000000000000000 ) ) ;
#1586 = DIRECTION ( 'NONE',  ( -1.000000000000000000, -0.000000000000000000, -0.000000000000000000 ) ) ;
#1587 = DIRECTION ( 'NONE',  ( 0.000000000000000000, -1.156482317317870246E-16, 1.000000000000000000 ) ) ;
#1588 = CARTESIAN_POINT ( 'NONE',  ( -818.8285638327251945, 78.67432280806566780, -154.6235849673217899 ) ) ;
#1589 = VERTEX_POINT ( 'NONE', #7656 ) ;
#1590 = CARTESIAN_POINT ( 'NONE',  ( -795.0000000000047748, 112.0000000000007532, -124.6807709998042384 ) ) ;
#1591 = AXIS2_PLACEMENT_3D ( 'NONE', #3125, #11841, #445 ) ;
#1592 = ADVANCED_FACE ( 'NONE', ( #2099, #9451 ), #10284, .T. ) ;
#1593 = DIRECTION ( 'NONE',  ( 0.000000000000000000, -0.5000000000000018874, -0.8660254037844375974 ) ) ;
#1594 = LINE ( 'NONE', #8942, #5885 ) ;
#1595 = CARTESIAN_POINT ( 'NONE',  ( 0.000000000000000000, -58.00000000000000711, -126.4213562373094959 ) ) ;
#1596 = CARTESIAN_POINT ( 'NONE',  ( 19.98721147511798080, 181.3928720024498205, -123.7411646176790327 ) ) ;
#1597 = ORIENTED_EDGE ( 'NONE', *, *, #6226, .T. ) ;
#1598 = ORIENTED_EDGE ( 'NONE', *, *, #5093, .T. ) ;
#1599 = LINE ( 'NONE', #10711, #846 ) ;
#1600 = CARTESIAN_POINT ( 'NONE',  ( 8.500000000000010658, 25.00000000000002132, -126.4213562373094959 ) ) ;
#1601 = CARTESIAN_POINT ( 'NONE',  ( -1046.909978542192675, 84.99913997988247161, -154.2940595301286919 ) ) ;
#1602 = CARTESIAN_POINT ( 'NONE',  ( -828.7636281597818879, 77.85463023298339635, -144.2471423470013576 ) ) ;
#1603 = CARTESIAN_POINT ( 'NONE',  ( 1.875296586882326249E-12, 0.000000000000000000, 46.07864376269049700 ) ) ;
#1604 = CARTESIAN_POINT ( 'NONE',  ( 0.09252763182291810773, 6.914127053141843504, -6.024380653971841859 ) ) ;
#1605 = CARTESIAN_POINT ( 'NONE',  ( -1012.226803665787770, 93.06815595962714838, -154.2940595301283224 ) ) ;
#1606 = PLANE ( 'NONE',  #8199 ) ;
#1607 = ORIENTED_EDGE ( 'NONE', *, *, #8386, .T. ) ;
#1608 = LINE ( 'NONE', #7425, #3319 ) ;
#1609 = CIRCLE ( 'NONE', #4593, 1.000000000000000888 ) ;
#1610 = ADVANCED_FACE ( 'NONE', ( #9701 ), #8887, .F. ) ;
#1611 = VERTEX_POINT ( 'NONE', #9641 ) ;
#1612 = CARTESIAN_POINT ( 'NONE',  ( -1016.652307257396728, 63.31440937415337800, -146.0307792196454102 ) ) ;
#1613 = EDGE_CURVE ( 'NONE', #4601, #7504, #3029, .T. ) ;
#1614 = DIRECTION ( 'NONE',  ( -0.000000000000000000, 1.000000000000000000, 7.930164461608263644E-17 ) ) ;
#1615 = VERTEX_POINT ( 'NONE', #11629 ) ;
#1616 = B_SPLINE_CURVE_WITH_KNOTS ( 'NONE', 3,
 ( #6872, #8786, #8954, #10641, #486, #2180, #7983, #5942, #11640, #7925, #10697, #11695, #2292, #11813, #6061, #6302, #6247, #1667, #7235, #8300, #7172, #1741, #8233, #11000, #9079, #9208, #3329, #5429, #8103, #10872, #4390, #9141, #3508, #2528, #814, #744, #7109, #1602, #2408, #2653, #4333, #2471 ),
 .UNSPECIFIED., .F., .F.,
 ( 4, 2, 2, 2, 2, 2, 2, 2, 2, 2, 2, 2, 2, 2, 2, 2, 2, 2, 2, 2, 4 ),
 ( 0.000000000000000000, 0.0009975002171434010391, 0.001496250325715081392, 0.001995000434286762180, 0.002992500651430000155, 0.003990000868573238997, 0.004987501085716477406, 0.005486251194287953062, 0.005985001302859429585, 0.006982501520002396510, 0.007980001737145364302, 0.008478751845717013430, 0.008977501954288664293, 0.009975002171431972958, 0.01097250238857527989, 0.01197000260571858508, 0.01296750282286189375, 0.01396500304000520068, 0.01496250325714850934, 0.01546125336572015327, 0.01596000347429179719 ),
 .UNSPECIFIED. ) ;
#1617 = ORIENTED_EDGE ( 'NONE', *, *, #4280, .F. ) ;
#1618 = VECTOR ( 'NONE', #6678, 1000.000000000000000 ) ;
#1619 = EDGE_CURVE ( 'NONE', #9863, #5323, #9346, .T. ) ;
#1620 = CARTESIAN_POINT ( 'NONE',  ( -19.97661686088444810, 180.0768701897325741, -126.1571822173844453 ) ) ;
#1621 = CARTESIAN_POINT ( 'NONE',  ( -154.5043356068770493, 12.00000000000000000, -102.0666613060160302 ) ) ;
#1622 = VERTEX_POINT ( 'NONE', #7855 ) ;
#1623 = CARTESIAN_POINT ( 'NONE',  ( -379.7747414317349808, 63.03754323421768646, -131.1733032197525119 ) ) ;
#1624 = CARTESIAN_POINT ( 'NONE',  ( -59.99999999999998579, 24.00000000000001421, -126.4213562373090696 ) ) ;
#1625 = ORIENTED_EDGE ( 'NONE', *, *, #7440, .F. ) ;
#1626 = ORIENTED_EDGE ( 'NONE', *, *, #1246, .F. ) ;
#1627 = CIRCLE ( 'NONE', #5771, 7.500000000000005329 ) ;
#1628 = CARTESIAN_POINT ( 'NONE',  ( -1057.805062346506702, 42.77845103615944566, -130.5712005305404944 ) ) ;
#1629 = FACE_OUTER_BOUND ( 'NONE', #9194, .T. ) ;
#1630 = ADVANCED_FACE ( 'NONE', ( #6917 ), #5866, .T. ) ;
#1631 = CARTESIAN_POINT ( 'NONE',  ( 1.561981751485805177E-12, 152.0000000000000000, 23.57864376269051832 ) ) ;
#1632 = CARTESIAN_POINT ( 'NONE',  ( -952.9945178120592573, 87.05516224832913963, -94.48732055948602238 ) ) ;
#1633 = CARTESIAN_POINT ( 'NONE',  ( -823.8285638327242850, 78.67432280806536937, -90.68077099980378364 ) ) ;
#1634 = ADVANCED_FACE ( 'NONE', ( #1303, #5056 ), #11683, .T. ) ;
#1635 = CARTESIAN_POINT ( 'NONE',  ( -384.9998751003590201, 83.30729021256857436, -104.6803604098840168 ) ) ;
#1636 = ORIENTED_EDGE ( 'NONE', *, *, #1312, .F. ) ;
#1637 = DIRECTION ( 'NONE',  ( 0.000000000000000000, 0.9467162604879117982, -0.3220688158263456113 ) ) ;
#1638 = DIRECTION ( 'NONE',  ( 0.9373521544934636518, 2.869494331159886689E-17, 0.3483833211657269557 ) ) ;
#1639 = CARTESIAN_POINT ( 'NONE',  ( 151.3258811035896656, 12.00000000000000000, -56.13263083939798292 ) ) ;
#1640 = VERTEX_POINT ( 'NONE', #6105 ) ;
#1641 = CARTESIAN_POINT ( 'NONE',  ( -975.1903095749676140, 79.73237568579435219, -94.48732055948607922 ) ) ;
#1642 = AXIS2_PLACEMENT_3D ( 'NONE', #6288, #7280, #1721 ) ;
#1643 = FACE_OUTER_BOUND ( 'NONE', #480, .T. ) ;
#1644 = CYLINDRICAL_SURFACE ( 'NONE', #11719, 134.9999999999999716 ) ;
#1645 = EDGE_CURVE ( 'NONE', #8550, #1954, #6674, .T. ) ;
#1646 = FACE_OUTER_BOUND ( 'NONE', #8624, .T. ) ;
#1647 = DIRECTION ( 'NONE',  ( 1.000000000000000000, 0.000000000000000000, 0.000000000000000000 ) ) ;
#1648 = CARTESIAN_POINT ( 'NONE',  ( -19.96447914003645607, 179.6944185909774490, -123.2758706440192213 ) ) ;
#1649 = CARTESIAN_POINT ( 'NONE',  ( -822.1849787629541879, 73.94083650471891644, -142.9856651621327046 ) ) ;
#1650 = AXIS2_PLACEMENT_3D ( 'NONE', #6841, #10610, #2149 ) ;
#1651 = ORIENTED_EDGE ( 'NONE', *, *, #3988, .F. ) ;
#1652 = CARTESIAN_POINT ( 'NONE',  ( -370.0238914150202731, 56.07874637648789928, -129.5483826961032037 ) ) ;
#1653 = ITEM_DEFINED_TRANSFORMATION ( 'NONE', 'NONE', #8615,  #11957 ) ;
#1654 = VERTEX_POINT ( 'NONE', #1583 ) ;
#1655 = CARTESIAN_POINT ( 'NONE',  ( -1030.931480980269043, 117.9615145441170654, -122.7172756069790722 ) ) ;
#1656 = DIRECTION ( 'NONE',  ( 0.000000000000000000, -1.000000000000000000, -4.625929269271452387E-16 ) ) ;
#1657 = CYLINDRICAL_SURFACE ( 'NONE', #6275, 7.500000000000007105 ) ;
#1658 = CARTESIAN_POINT ( 'NONE',  ( 35.00000000000000000, 81.99999999999998579, 190.3192290001959748 ) ) ;
#1659 = CIRCLE ( 'NONE', #8766, 1.000000000000000888 ) ;
#1660 = AXIS2_PLACEMENT_3D ( 'NONE', #172, #6791, #5799 ) ;
#1661 = CARTESIAN_POINT ( 'NONE',  ( 19.99452644844618732, 181.5558364952455577, -124.0087194824425865 ) ) ;
#1662 = ORIENTED_EDGE ( 'NONE', *, *, #4942, .F. ) ;
#1663 = EDGE_LOOP ( 'NONE', ( #9512, #6396, #1868, #515 ) ) ;
#1664 = DIRECTION ( 'NONE',  ( -0.000000000000000000, -1.000000000000000000, -0.000000000000000000 ) ) ;
#1665 = DIRECTION ( 'NONE',  ( 0.000000000000000000, 0.000000000000000000, 1.000000000000000000 ) ) ;
#1666 = CARTESIAN_POINT ( 'NONE',  ( -1046.457602311632627, 98.67849639484583690, -149.7857175106632894 ) ) ;
#1667 = CARTESIAN_POINT ( 'NONE',  ( -822.1849787629572575, 73.94083650471947067, -142.9856651621330457 ) ) ;
#1668 = AXIS2_PLACEMENT_3D ( 'NONE', #4762, #7721, #9401 ) ;
#1669 = CARTESIAN_POINT ( 'NONE',  ( -823.8285638327247398, 78.67432280806536937, -158.6807709998041673 ) ) ;
#1670 = LINE ( 'NONE', #3569, #9944 ) ;
#1671 = AXIS2_PLACEMENT_3D ( 'NONE', #8007, #9792, #8865 ) ;
#1672 = CARTESIAN_POINT ( 'NONE',  ( -994.1998135634695473, 88.30642396300672203, -154.2940595301282656 ) ) ;
#1673 = FACE_OUTER_BOUND ( 'NONE', #5768, .T. ) ;
#1674 = ORIENTED_EDGE ( 'NONE', *, *, #10837, .F. ) ;
#1675 = CARTESIAN_POINT ( 'NONE',  ( 1.561981751485805177E-12, -6.000000000000006217, 31.07864376269051121 ) ) ;
#1676 =( LENGTH_UNIT ( ) NAMED_UNIT ( * ) SI_UNIT ( .MILLI., .METRE. ) );
#1677 = ORIENTED_EDGE ( 'NONE', *, *, #12039, .T. ) ;
#1678 = DIRECTION ( 'NONE',  ( 0.000000000000000000, 0.000000000000000000, 1.000000000000000000 ) ) ;
#1679 = CARTESIAN_POINT ( 'NONE',  ( -927.8303129675907712, 79.95948428978974221, -152.5758913445291682 ) ) ;
#1680 = CARTESIAN_POINT ( 'NONE',  ( 19.99999999999986855, 182.7144438187336277, -124.9030158930556667 ) ) ;
#1681 = ORIENTED_EDGE ( 'NONE', *, *, #11312, .T. ) ;
#1682 = AXIS2_PLACEMENT_3D ( 'NONE', #5167, #3665, #703 ) ;
#1683 = AXIS2_PLACEMENT_3D ( 'NONE', #3512, #2593, #6365 ) ;
#1684 = ORIENTED_EDGE ( 'NONE', *, *, #11803, .T. ) ;
#1685 = ADVANCED_FACE ( 'NONE', ( #9060 ), #595, .T. ) ;
#1686 = EDGE_CURVE ( 'NONE', #192, #10150, #2698, .T. ) ;
#1687 = EDGE_LOOP ( 'NONE', ( #5931, #3580 ) ) ;
#1688 = CARTESIAN_POINT ( 'NONE',  ( -370.1689562966705580, 56.44580195161717029, -131.5601801359200920 ) ) ;
#1689 = DIRECTION ( 'NONE',  ( -8.163404592832030268E-17, 1.000000000000000000, -0.000000000000000000 ) ) ;
#1690 = VERTEX_POINT ( 'NONE', #10112 ) ;
#1691 = AXIS2_PLACEMENT_3D ( 'NONE', #11611, #2622, #6400 ) ;
#1692 = EDGE_CURVE ( 'NONE', #11672, #7759, #8013, .T. ) ;
#1693 = CYLINDRICAL_SURFACE ( 'NONE', #8004, 1.500000000000000444 ) ;
#1694 = DIRECTION ( 'NONE',  ( 0.000000000000000000, 0.000000000000000000, 1.000000000000000000 ) ) ;
#1695 = CARTESIAN_POINT ( 'NONE',  ( 21.06714599819344258, 179.1261101450867557, -125.9628648169738625 ) ) ;
#1696 = CARTESIAN_POINT ( 'NONE',  ( -818.8285638327251945, 78.67432280806566780, -154.6235849673217899 ) ) ;
#1697 = AXIS2_PLACEMENT_3D ( 'NONE', #11285, #1638, #9307 ) ;
#1698 = CARTESIAN_POINT ( 'NONE',  ( -795.0000000000004547, 76.10956187831470743, -95.06748246948018277 ) ) ;
#1699 = LINE ( 'NONE', #7261, #4772 ) ;
#1700 = CARTESIAN_POINT ( 'NONE',  ( -1065.000000000003865, 52.00000000000021316, -126.6442663926290493 ) ) ;
#1701 = EDGE_CURVE ( 'NONE', #6923, #10076, #8157, .T. ) ;
#1702 = VERTEX_POINT ( 'NONE', #9184 ) ;
#1703 = LINE ( 'NONE', #916, #11145 ) ;
#1704 = EDGE_CURVE ( 'NONE', #6191, #9127, #4013, .T. ) ;
#1705 = DIRECTION ( 'NONE',  ( 0.000000000000000000, 0.000000000000000000, 1.000000000000000000 ) ) ;
#1706 = CARTESIAN_POINT ( 'NONE',  ( 35.00000000000000000, 12.00000000000000000, 81.78351099501843180 ) ) ;
#1707 = CARTESIAN_POINT ( 'NONE',  ( -82.49999999999998579, 152.0000000000000000, -126.4213562373088564 ) ) ;
#1708 = VERTEX_POINT ( 'NONE', #11240 ) ;
#1709 = FACE_OUTER_BOUND ( 'NONE', #4848, .T. ) ;
#1710 = CARTESIAN_POINT ( 'NONE',  ( -952.9945178120592573, 87.05516224832913963, -94.48732055948602238 ) ) ;
#1711 = FACE_BOUND ( 'NONE', #6862, .T. ) ;
#1712 = ORIENTED_EDGE ( 'NONE', *, *, #6388, .F. ) ;
#1713 = CARTESIAN_POINT ( 'NONE',  ( 0.000000000000000000, 12.00000000000000000, -89.68077099980401101 ) ) ;
#1714 = CARTESIAN_POINT ( 'NONE',  ( 19.86348653241994100, 179.0685786869776450, -127.0149889656965740 ) ) ;
#1715 = AXIS2_PLACEMENT_3D ( 'NONE', #7182, #3409, #3235 ) ;
#1716 = APPLICATION_CONTEXT ( 'automotive_design' ) ;
#1717 = CARTESIAN_POINT ( 'NONE',  ( -822.1919554870369211, 73.93830887977112809, -106.3769876045755467 ) ) ;
#1718 = CARTESIAN_POINT ( 'NONE',  ( -826.9024563477383936, 74.71743289348825101, -143.3087845970614183 ) ) ;
#1719 = ORIENTED_EDGE ( 'NONE', *, *, #8523, .F. ) ;
#1720 = ORIENTED_EDGE ( 'NONE', *, *, #564, .T. ) ;
#1721 = DIRECTION ( 'NONE',  ( 0.000000000000000000, 0.000000000000000000, 1.000000000000000000 ) ) ;
#1722 = CONTEXT_DEPENDENT_SHAPE_REPRESENTATION ( #8031, #11583 ) ;
#1723 = CARTESIAN_POINT ( 'NONE',  ( -374.0275851353517851, 95.01260271039970462, -109.3552309949570400 ) ) ;
#1724 = CARTESIAN_POINT ( 'NONE',  ( 35.00000000000000000, 164.0000000000000000, -124.6807709998038689 ) ) ;
#1725 = AXIS2_PLACEMENT_3D ( 'NONE', #2506, #656, #3488 ) ;
#1726 = EDGE_CURVE ( 'NONE', #5232, #609, #4808, .T. ) ;
#1727 = ORIENTED_EDGE ( 'NONE', *, *, #11837, .F. ) ;
#1728 = FACE_BOUND ( 'NONE', #8840, .T. ) ;
#1729 = CARTESIAN_POINT ( 'NONE',  ( -991.5701548301638013, 122.8678427087060214, -122.7172756069787170 ) ) ;
#1730 = CARTESIAN_POINT ( 'NONE',  ( -22.49999999999999289, 139.9999999999999716, -126.4213562373092685 ) ) ;
#1731 = CARTESIAN_POINT ( 'NONE',  ( 19.92971727147881467, 178.2306503425758990, -126.3637072540984292 ) ) ;
#1732 = DIRECTION ( 'NONE',  ( 0.000000000000000000, 0.000000000000000000, -1.000000000000000000 ) ) ;
#1733 = CARTESIAN_POINT ( 'NONE',  ( 20.00016885954969226, 181.6903612530189491, -124.3916023546908463 ) ) ;
#1734 = CIRCLE ( 'NONE', #3292, 5.035999999999999588 ) ;
#1735 = VERTEX_POINT ( 'NONE', #12032 ) ;
#1736 = CIRCLE ( 'NONE', #11795, 7.500000000000007994 ) ;
#1737 = ORIENTED_EDGE ( 'NONE', *, *, #7538, .T. ) ;
#1738 = DIRECTION ( 'NONE',  ( 0.000000000000000000, 0.000000000000000000, 1.000000000000000000 ) ) ;
#1739 = CARTESIAN_POINT ( 'NONE',  ( 21.06635469844951558, 179.5529625613920643, -126.2817468820535964 ) ) ;
#1740 = CARTESIAN_POINT ( 'NONE',  ( -1065.000000000003638, 87.89043812168645786, -154.2940595301284361 ) ) ;
#1741 = CARTESIAN_POINT ( 'NONE',  ( -823.9892610140105944, 73.67413949648602056, -142.8653811665928686 ) ) ;
#1742 = DIRECTION ( 'NONE',  ( -0.000000000000000000, 1.000000000000000000, -0.000000000000000000 ) ) ;
#1743 = FACE_OUTER_BOUND ( 'NONE', #3927, .T. ) ;
#1744 = ORIENTED_EDGE ( 'NONE', *, *, #860, .F. ) ;
#1745 = TOROIDAL_SURFACE ( 'NONE', #10019, 6.500000000000005329, 1.000000000000000000 ) ;
#1746 = CARTESIAN_POINT ( 'NONE',  ( -374.4050532074698481, 92.42149850801368416, -141.8266576912406833 ) ) ;
#1747 = ORIENTED_EDGE ( 'NONE', *, *, #11277, .F. ) ;
#1748 = CARTESIAN_POINT ( 'NONE',  ( -1056.430032577873362, 71.19035303699479300, -154.2940595301283793 ) ) ;
#1749 = CARTESIAN_POINT ( 'NONE',  ( 1.250503886288004501E-12, -6.000000000000004441, -13.92135623730950478 ) ) ;
#1750 = EDGE_LOOP ( 'NONE', ( #6442, #1267 ) ) ;
#1751 = AXIS2_PLACEMENT_3D ( 'NONE', #7084, #2387, #3243 ) ;
#1752 = AXIS2_PLACEMENT_3D ( 'NONE', #8038, #540, #7288 ) ;
#1753 = FACE_OUTER_BOUND ( 'NONE', #5904, .T. ) ;
#1754 = CARTESIAN_POINT ( 'NONE',  ( 6.247927005943220505E-13, 12.00000000000000000, -66.42135623730949590 ) ) ;
#1755 = ORIENTED_EDGE ( 'NONE', *, *, #4932, .T. ) ;
#1756 = CARTESIAN_POINT ( 'NONE',  ( -374.0178982243409109, 68.97857190266184091, -139.9467288357900827 ) ) ;
#1757 = DIRECTION ( 'NONE',  ( -0.000000000000000000, 1.000000000000000000, 0.000000000000000000 ) ) ;
#1758 = DIRECTION ( 'NONE',  ( 1.000000000000000000, -1.262554838833776231E-16, 0.000000000000000000 ) ) ;
#1759 = VECTOR ( 'NONE', #7848, 1000.000000000000000 ) ;
#1760 = VECTOR ( 'NONE', #8649, 1000.000000000000000 ) ;
#1761 = EDGE_CURVE ( 'NONE', #10791, #8166, #4560, .T. ) ;
#1762 = CARTESIAN_POINT ( 'NONE',  ( -305.0000000000000568, 139.9999999999999716, -89.68077099980384048 ) ) ;
#1763 = CARTESIAN_POINT ( 'NONE',  ( 0.09318607064769238169, 1.767053008364804834, 9.000000000000000000 ) ) ;
#1764 = CARTESIAN_POINT ( 'NONE',  ( 1.874378101782966050E-12, 12.00000000000000000, 61.07864376269051121 ) ) ;
#1765 = CARTESIAN_POINT ( 'NONE',  ( -821.0802431487063586, 81.36881375820571805, -95.06748246948008330 ) ) ;
#1766 = CIRCLE ( 'NONE', #1563, 7.500000000000007105 ) ;
#1767 = CARTESIAN_POINT ( 'NONE',  ( -59.99999999999998579, 12.00000000000001421, -126.4213562373090696 ) ) ;
#1768 = CARTESIAN_POINT ( 'NONE',  ( -901.8785362142589292, 56.55314031071017666, -126.6442663926291061 ) ) ;
#1769 = CARTESIAN_POINT ( 'NONE',  ( -826.8836092318815645, 82.64591421739883970, -144.6711677827317430 ) ) ;
#1770 = ORIENTED_EDGE ( 'NONE', *, *, #2177, .T. ) ;
#1771 = CARTESIAN_POINT ( 'NONE',  ( -828.3910170805050939, 80.72627522873268902, -144.6407408995347339 ) ) ;
#1772 = CARTESIAN_POINT ( 'NONE',  ( 0.000000000000000000, 0.000000000000000000, 0.000000000000000000 ) ) ;
#1773 = ORIENTED_EDGE ( 'NONE', *, *, #6240, .T. ) ;
#1774 = DIRECTION ( 'NONE',  ( -1.186840563529527301E-16, 1.000000000000000000, -0.000000000000000000 ) ) ;
#1775 = CARTESIAN_POINT ( 'NONE',  ( -818.6751755801135459, 47.70925804672316417, -99.57582448894514471 ) ) ;
#1776 = CARTESIAN_POINT ( 'NONE',  ( 6.899999999999999467, 8.999999999999998224, 0.000000000000000000 ) ) ;
#1777 = AXIS2_PLACEMENT_3D ( 'NONE', #9816, #356, #6913 ) ;
#1778 = DIRECTION ( 'NONE',  ( 0.000000000000000000, 1.000000000000000000, 6.938893903907169213E-16 ) ) ;
#1779 = DIRECTION ( 'NONE',  ( -0.000000000000000000, -7.930164461608263644E-17, 1.000000000000000000 ) ) ;
#1780 = ADVANCED_FACE ( 'NONE', ( #11041 ), #6470, .F. ) ;
#1781 = CYLINDRICAL_SURFACE ( 'NONE', #8687, 7.500000000000007994 ) ;
#1782 = CARTESIAN_POINT ( 'NONE',  ( -20.00091651665146841, 178.6995461844927888, -124.4414934301431401 ) ) ;
#1783 = CARTESIAN_POINT ( 'NONE',  ( -828.8285638327206470, 78.67432280806529832, -144.4023295390027215 ) ) ;
#1784 = ORIENTED_EDGE ( 'NONE', *, *, #8193, .F. ) ;
#1785 = EDGE_LOOP ( 'NONE', ( #8641, #2412, #6566 ) ) ;
#1786 = CARTESIAN_POINT ( 'NONE',  ( -371.8534480886071378, 61.21526739536749773, -143.1506241535973061 ) ) ;
#1787 = CONTEXT_DEPENDENT_SHAPE_REPRESENTATION ( #5666, #9703 ) ;
#1788 = ORIENTED_EDGE ( 'NONE', *, *, #5842, .T. ) ;
#1789 = DIRECTION ( 'NONE',  ( -1.000000000000000000, -0.000000000000000000, -0.000000000000000000 ) ) ;
#1790 = EDGE_CURVE ( 'NONE', #7713, #882, #657, .T. ) ;
#1791 = CARTESIAN_POINT ( 'NONE',  ( 19.96940092271958278, 182.5175105289615942, -125.7966324820120008 ) ) ;
#1792 = EDGE_CURVE ( 'NONE', #10730, #2533, #9136, .T. ) ;
#1793 = ORIENTED_EDGE ( 'NONE', *, *, #6606, .F. ) ;
#1794 = EDGE_CURVE ( 'NONE', #6737, #10573, #4624, .T. ) ;
#1795 = CYLINDRICAL_SURFACE ( 'NONE', #10448, 7.500000000000007105 ) ;
#1796 = DIRECTION ( 'NONE',  ( 0.000000000000000000, 0.000000000000000000, 1.000000000000000000 ) ) ;
#1797 = CARTESIAN_POINT ( 'NONE',  ( -1061.468168685229102, 92.73456844357778550, -152.5758913445291398 ) ) ;
#1798 = CARTESIAN_POINT ( 'NONE',  ( -372.7288769611630528, 100.8944622026212983, -118.0665564160781855 ) ) ;
#1799 = EDGE_CURVE ( 'NONE', #9710, #8281, #1442, .T. ) ;
#1800 = SURFACE_SIDE_STYLE ('',( #681 ) ) ;
#1801 = CARTESIAN_POINT ( 'NONE',  ( -6.500766111939939161E-15, 7.573738413550457516, -4.881900264494495545 ) ) ;
#1802 = CYLINDRICAL_SURFACE ( 'NONE', #6617, 7.500000000000007105 ) ;
#1803 = ORIENTED_EDGE ( 'NONE', *, *, #8190, .F. ) ;
#1804 = FACE_BOUND ( 'NONE', #4441, .T. ) ;
#1805 = CARTESIAN_POINT ( 'NONE',  ( -382.1275881780431973, 96.19125754664578665, -138.8335771761920796 ) ) ;
#1806 = PRODUCT_DEFINITION_SHAPE ( 'NONE', 'NONE',  #3674 ) ;
#1807 = ORIENTED_EDGE ( 'NONE', *, *, #7454, .T. ) ;
#1808 = CARTESIAN_POINT ( 'NONE',  ( -1015.517346982278013, 86.95624952299075971, -154.8742214401231649 ) ) ;
#1809 = CARTESIAN_POINT ( 'NONE',  ( -795.0000000000040927, 111.6133447792292088, -130.5712005305403522 ) ) ;
#1810 = VERTEX_POINT ( 'NONE', #5344 ) ;
#1811 = AXIS2_PLACEMENT_3D ( 'NONE', #11030, #711, #11893 ) ;
#1812 = ADVANCED_FACE ( 'NONE', ( #10178 ), #1644, .F. ) ;
#1813 = VERTEX_POINT ( 'NONE', #5472 ) ;
#1814 = CARTESIAN_POINT ( 'NONE',  ( -19.99532149354086030, 181.6339454046986361, -125.1698373029890519 ) ) ;
#1815 = DIRECTION ( 'NONE',  ( 0.3117078928809249860, 1.670400663243698742E-14, -0.9501779778103330854 ) ) ;
#1816 = CIRCLE ( 'NONE', #8529, 7.500000000000007105 ) ;
#1817 = ORIENTED_EDGE ( 'NONE', *, *, #9085, .F. ) ;
#1818 = CARTESIAN_POINT ( 'NONE',  ( -381.5707893087703724, 66.54686343221263201, -137.3937270100335866 ) ) ;
#1819 = DIRECTION ( 'NONE',  ( 0.000000000000000000, 0.000000000000000000, 1.000000000000000000 ) ) ;
#1820 = DIRECTION ( 'NONE',  ( 0.000000000000000000, 0.000000000000000000, -1.000000000000000000 ) ) ;
#1821 = DIRECTION ( 'NONE',  ( -1.000000000000000000, 0.000000000000000000, 0.000000000000000000 ) ) ;
#1822 = ORIENTED_EDGE ( 'NONE', *, *, #2939, .F. ) ;
#1823 = DIRECTION ( 'NONE',  ( 1.000000000000000000, 0.000000000000000000, 0.000000000000000000 ) ) ;
#1824 = TOROIDAL_SURFACE ( 'NONE', #10885, 10.00000000000002487, 1.499999999999998002 ) ;
#1825 = DIRECTION ( 'NONE',  ( 0.000000000000000000, 0.000000000000000000, 1.000000000000000000 ) ) ;
#1826 = CARTESIAN_POINT ( 'NONE',  ( 19.99178670042469719, 178.8663240180210039, -125.3736306701222532 ) ) ;
#1827 = CARTESIAN_POINT ( 'NONE',  ( -954.0832773815070595, 60.15510303592672869, -103.3307627799632513 ) ) ;
#1828 = DIRECTION ( 'NONE',  ( 0.000000000000000000, 0.000000000000000000, 1.000000000000000000 ) ) ;
#1829 = DIRECTION ( 'NONE',  ( -3.061276722312011504E-17, 1.000000000000000000, 0.000000000000000000 ) ) ;
#1830 = CARTESIAN_POINT ( 'NONE',  ( -379.5881075290514559, 101.2865363140498403, -130.0868282690590831 ) ) ;
#1831 = EDGE_LOOP ( 'NONE', ( #6682, #7432 ) ) ;
#1832 = CARTESIAN_POINT ( 'NONE',  ( -820.4056028115145409, 82.32260517263510735, -144.6785023965173025 ) ) ;
#1833 = CARTESIAN_POINT ( 'NONE',  ( 9.981418654830825461E-15, 12.00000000000003908, 252.8427124746189918 ) ) ;
#1834 = CARTESIAN_POINT ( 'NONE',  ( -828.8285638327206470, 78.67432280806529832, -104.9592124606049879 ) ) ;
#1835 = VERTEX_POINT ( 'NONE', #2767 ) ;
#1836 = CARTESIAN_POINT ( 'NONE',  ( -1062.810894920125520, 52.92335929224832825, -107.9061927053327139 ) ) ;
#1837 = DIRECTION ( 'NONE',  ( 0.000000000000000000, 5.522905491341382306E-16, 1.000000000000000000 ) ) ;
#1838 = LINE ( 'NONE', #5602, #8379 ) ;
#1839 = VECTOR ( 'NONE', #9227, 1000.000000000000000 ) ;
#1840 = CARTESIAN_POINT ( 'NONE',  ( -926.6866529578969676, 120.3119365386820192, -107.9061927053322734 ) ) ;
#1841 = DIRECTION ( 'NONE',  ( -0.000000000000000000, -1.000000000000000000, -1.757987137413040192E-14 ) ) ;
#1842 = CARTESIAN_POINT ( 'NONE',  ( -20.91120072986939959, 178.8231192296793779, -124.2317959954639406 ) ) ;
#1843 = DIRECTION ( 'NONE',  ( 0.000000000000000000, 0.000000000000000000, 1.000000000000000000 ) ) ;
#1844 = EDGE_CURVE ( 'NONE', #1455, #7353, #10299, .T. ) ;
#1845 = ORIENTED_EDGE ( 'NONE', *, *, #3755, .F. ) ;
#1846 = DIRECTION ( 'NONE',  ( 0.000000000000000000, 1.000000000000000000, 0.000000000000000000 ) ) ;
#1847 = EDGE_CURVE ( 'NONE', #7181, #4605, #1838, .T. ) ;
#1848 = AXIS2_PLACEMENT_3D ( 'NONE', #4997, #2109, #4085 ) ;
#1849 = ORIENTED_EDGE ( 'NONE', *, *, #1121, .T. ) ;
#1850 = CARTESIAN_POINT ( 'NONE',  ( -795.0000000000002274, 107.1049510380560719, -107.9061927053326002 ) ) ;
#1851 = CARTESIAN_POINT ( 'NONE',  ( -141.4213562373095101, 0.000000000000000000, 3.644282033693712520E-14 ) ) ;
#1852 = ADVANCED_FACE ( 'NONE', ( #9118 ), #792, .F. ) ;
#1853 = CARTESIAN_POINT ( 'NONE',  ( 21.06610394755309201, 181.3758997718305181, -125.8629927389160486 ) ) ;
#1854 = CARTESIAN_POINT ( 'NONE',  ( 19.98052438014507715, 181.2452332506350672, -123.5813376981535043 ) ) ;
#1855 = VERTEX_POINT ( 'NONE', #855 ) ;
#1856 = VERTEX_POINT ( 'NONE', #9497 ) ;
#1857 = DIRECTION ( 'NONE',  ( -0.000000000000000000, -0.000000000000000000, 1.000000000000000000 ) ) ;
#1858 = DIRECTION ( 'NONE',  ( -0.9501779778103373042, 0.000000000000000000, 0.3117078928809121074 ) ) ;
#1859 = CARTESIAN_POINT ( 'NONE',  ( -794.9999999999980673, 87.89043812168634418, -154.2940595301278961 ) ) ;
#1860 = CARTESIAN_POINT ( 'NONE',  ( -305.0000000000000568, 81.99999999999995737, -89.68077099980384048 ) ) ;
#1861 = DIRECTION ( 'NONE',  ( 0.000000000000000000, 1.000000000000000000, 0.000000000000000000 ) ) ;
#1862 = CARTESIAN_POINT ( 'NONE',  ( -821.0802431487052218, 81.36881375820613016, -154.2940595301280382 ) ) ;
#1863 = VERTEX_POINT ( 'NONE', #10604 ) ;
#1864 = FACE_OUTER_BOUND ( 'NONE', #7942, .T. ) ;
#1865 = CARTESIAN_POINT ( 'NONE',  ( -172.5000000000000000, -9.213203435596478030, -126.4213562373082453 ) ) ;
#1866 = ADVANCED_FACE ( 'NONE', ( #974 ), #3805, .T. ) ;
#1867 = VECTOR ( 'NONE', #5188, 1000.000000000000000 ) ;
#1868 = ORIENTED_EDGE ( 'NONE', *, *, #2750, .T. ) ;
#1869 = CARTESIAN_POINT ( 'NONE',  ( -795.0000000000094360, 82.00000000000081002, -154.8742214401225397 ) ) ;
#1870 = AXIS2_PLACEMENT_3D ( 'NONE', #5794, #2163, #7715 ) ;
#1871 = ORIENTED_EDGE ( 'NONE', *, *, #2513, .T. ) ;
#1872 = PRODUCT_DEFINITION ( 'UNKNOWN', '', #5446, #1966 ) ;
#1873 = ORIENTED_EDGE ( 'NONE', *, *, #3334, .F. ) ;
#1874 = AXIS2_PLACEMENT_3D ( 'NONE', #1577, #6860, #4490 ) ;
#1875 = CARTESIAN_POINT ( 'NONE',  ( -828.5766943389870676, 80.27470094935115696, -144.6085013259159098 ) ) ;
#1876 = CARTESIAN_POINT ( 'NONE',  ( -20.87666491430435300, 181.4765249126461129, -124.0391332007959306 ) ) ;
#1877 = CARTESIAN_POINT ( 'NONE',  ( 8.099999999999999645, 0.000000000000000000, 0.000000000000000000 ) ) ;
#1878 = CARTESIAN_POINT ( 'NONE',  ( -1025.595947590964442, 58.17469240935094632, -141.4553492942760329 ) ) ;
#1879 = ORIENTED_EDGE ( 'NONE', *, *, #6839, .T. ) ;
#1880 = CARTESIAN_POINT ( 'NONE',  ( -374.3481803600093372, 71.08267651485977012, -141.5671192069848701 ) ) ;
#1881 = DIRECTION ( 'NONE',  ( 1.000000000000000000, 0.000000000000000000, 0.000000000000000000 ) ) ;
#1882 = CARTESIAN_POINT ( 'NONE',  ( -384.7075901990183411, 77.40006559035658995, -105.2059176660476396 ) ) ;
#1884 = EDGE_CURVE ( 'NONE', #8131, #5617, #61, .T. ) ;
#1883 = DIRECTION ( 'NONE',  ( 0.000000000000000000, -1.000000000000000000, -4.625929269271452387E-16 ) ) ;
#1885 = ORIENTED_EDGE ( 'NONE', *, *, #5319, .F. ) ;
#1886 = AXIS2_PLACEMENT_3D ( 'NONE', #3034, #893, #9591 ) ;
#1887 = VECTOR ( 'NONE', #3375, 1000.000000000000000 ) ;
#1888 = CARTESIAN_POINT ( 'NONE',  ( -240.0000000000000000, 151.9999999999999716, -126.4213562373078190 ) ) ;
#1889 = DIRECTION ( 'NONE',  ( 0.000000000000000000, 1.000000000000000000, 2.312964634635740689E-15 ) ) ;
#1890 = CARTESIAN_POINT ( 'NONE',  ( -1020.755281158177013, 68.40999151392674094, -99.57582448894541471 ) ) ;
#1891 = CARTESIAN_POINT ( 'NONE',  ( -820.5194676126043305, 82.43685310047874282, -104.6842045117120534 ) ) ;
#1892 = CARTESIAN_POINT ( 'NONE',  ( -819.8521517457915024, 81.72352651608187557, -144.6807563939349848 ) ) ;
#1893 = MECHANICAL_DESIGN_GEOMETRIC_PRESENTATION_REPRESENTATION (  '', ( #3255 ), #10179 ) ;
#1894 = EDGE_LOOP ( 'NONE', ( #5076, #264, #7551, #11726, #10183, #6058 ) ) ;
#1895 = FACE_BOUND ( 'NONE', #6123, .T. ) ;
#1896 = CARTESIAN_POINT ( 'NONE',  ( -126.4213562373094959, -485.4999999999998863, 2.081668171172168513E-14 ) ) ;
#1897 = CARTESIAN_POINT ( 'NONE',  ( -373.6479907027180616, 95.69918402684290015, -99.08269489361265414 ) ) ;
#1898 = EDGE_LOOP ( 'NONE', ( #2480, #3346, #2420, #11357 ) ) ;
#1899 = CARTESIAN_POINT ( 'NONE',  ( -1065.000000000007049, 56.89504896194527106, -107.9061927053324581 ) ) ;
#1900 = LINE ( 'NONE', #3063, #9448 ) ;
#1901 = CARTESIAN_POINT ( 'NONE',  ( -7.500000000000004441, 25.00000000000002132, -126.4213562373094959 ) ) ;
#1902 = FACE_OUTER_BOUND ( 'NONE', #925, .T. ) ;
#1903 = ORIENTED_EDGE ( 'NONE', *, *, #2818, .T. ) ;
#1904 = CARTESIAN_POINT ( 'NONE',  ( -6.499999999999979572, -7.999999999999979572, -124.6807709998038405 ) ) ;
#1905 = CONTEXT_DEPENDENT_SHAPE_REPRESENTATION ( #12051, #1220 ) ;
#1906 = CARTESIAN_POINT ( 'NONE',  ( -374.7132803760889601, 89.60697909709962516, -106.0899807314232248 ) ) ;
#1907 = ORIENTED_EDGE ( 'NONE', *, *, #6600, .F. ) ;
#1908 = CARTESIAN_POINT ( 'NONE',  ( -926.5908784743340902, 123.4113341959661767, -113.1262384684093831 ) ) ;
#1909 = AXIS2_PLACEMENT_3D ( 'NONE', #1145, #4899, #3790 ) ;
#1910 = DIRECTION ( 'NONE',  ( -8.163404592832031500E-17, 1.000000000000000000, 0.000000000000000000 ) ) ;
#1911 = ADVANCED_FACE ( 'NONE', ( #1039 ), #3814, .T. ) ;
#1912 = CARTESIAN_POINT ( 'NONE',  ( -19.92695522958598175, 181.7999794737119430, -122.9644587262777549 ) ) ;
#1913 = ORIENTED_EDGE ( 'NONE', *, *, #824, .F. ) ;
#1914 = DIRECTION ( 'NONE',  ( -8.163404592832030268E-17, 1.000000000000000000, -0.000000000000000000 ) ) ;
#1915 = AXIS2_PLACEMENT_3D ( 'NONE', #4118, #3178, #2808 ) ;
#1916 = CARTESIAN_POINT ( 'NONE',  ( -112.4999999999999858, 152.0000000000000000, -126.4213562373086575 ) ) ;
#1917 = DIRECTION ( 'NONE',  ( -0.000000000000000000, 0.000000000000000000, 1.000000000000000000 ) ) ;
#1918 = CARTESIAN_POINT ( 'NONE',  ( -1037.550865396555764, 105.7975851359348667, -146.0307792196445860 ) ) ;
#1919 = DIRECTION ( 'NONE',  ( 0.000000000000000000, 0.000000000000000000, 1.000000000000000000 ) ) ;
#1920 = FACE_OUTER_BOUND ( 'NONE', #183, .T. ) ;
#1921 = CARTESIAN_POINT ( 'NONE',  ( 126.4213562373094959, -494.9999999999998863, -7.500000000000019540 ) ) ;
#1922 = DIRECTION ( 'NONE',  ( 0.000000000000000000, 0.000000000000000000, -1.000000000000000000 ) ) ;
#1923 = EDGE_LOOP ( 'NONE', ( #6325, #7312 ) ) ;
#1924 = CARTESIAN_POINT ( 'NONE',  ( -374.6521690518432024, 90.20916286035372877, -142.9852835970012279 ) ) ;
#1925 = ORIENTED_EDGE ( 'NONE', *, *, #2302, .F. ) ;
#1926 = CARTESIAN_POINT ( 'NONE',  ( -1046.909978542192675, 84.99913997988247161, -154.2940595301286919 ) ) ;
#1927 = CIRCLE ( 'NONE', #5071, 7.500000000000012434 ) ;
#1928 = DIRECTION ( 'NONE',  ( 0.000000000000000000, 0.000000000000000000, 1.000000000000000000 ) ) ;
#1929 = EDGE_CURVE ( 'NONE', #9223, #6290, #4213, .T. ) ;
#1930 = EDGE_LOOP ( 'NONE', ( #1720, #11297, #5027, #837 ) ) ;
#1931 = ORIENTED_EDGE ( 'NONE', *, *, #4795, .T. ) ;
#1932 = EDGE_CURVE ( 'NONE', #11819, #8540, #4406, .T. ) ;
#1933 = CARTESIAN_POINT ( 'NONE',  ( -827.8097080315070571, 81.71711720835189396, -144.6806456489627806 ) ) ;
#1934 = CARTESIAN_POINT ( 'NONE',  ( -19.93883021351429363, 182.2592841156773602, -126.2495949291102022 ) ) ;
#1935 = FACE_OUTER_BOUND ( 'NONE', #4634, .T. ) ;
#1936 = VERTEX_POINT ( 'NONE', #12233 ) ;
#1937 = STYLED_ITEM ( 'NONE', ( #3274 ), #8029 ) ;
#1938 = CARTESIAN_POINT ( 'NONE',  ( -385.0061886013530739, 82.02011007860102154, -144.6917801619403861 ) ) ;
#1939 = DIRECTION ( 'NONE',  ( 0.000000000000000000, -1.000000000000000000, -1.669238443041288415E-16 ) ) ;
#1940 = CARTESIAN_POINT ( 'NONE',  ( -374.7231203874862331, 74.61313258587077257, -106.0425182818924554 ) ) ;
#1941 = DIRECTION ( 'NONE',  ( -0.7071067811865479058, 0.000000000000000000, -0.7071067811865472397 ) ) ;
#1942 = AXIS2_PLACEMENT_3D ( 'NONE', #4530, #6845, #6192 ) ;
#1943 = EDGE_CURVE ( 'NONE', #338, #9776, #5982, .T. ) ;
#1944 = DIRECTION ( 'NONE',  ( 0.000000000000000000, 0.000000000000000000, 1.000000000000000000 ) ) ;
#1945 = DIRECTION ( 'NONE',  ( -1.000000000000000000, -3.061276722312011504E-17, 0.000000000000000000 ) ) ;
#1946 = ADVANCED_FACE ( 'NONE', ( #11248 ), #2636, .T. ) ;
#1947 = CARTESIAN_POINT ( 'NONE',  ( -927.8303129675875880, 79.95948428978934430, -96.78565065507952170 ) ) ;
#1948 = CARTESIAN_POINT ( 'NONE',  ( -3.506716401632803404E-15, -7.351593252548093815, -5.266666970006169457 ) ) ;
#1949 = CARTESIAN_POINT ( 'NONE',  ( 7.500000000000000000, 1.102182119232617517E-15, -8.999999999999998224 ) ) ;
#1950 = CARTESIAN_POINT ( 'NONE',  ( -1014.107508992743988, 52.59077491224116585, -130.5712005305404944 ) ) ;
#1951 = CARTESIAN_POINT ( 'NONE',  ( -821.3235167497211933, 83.01396457509433446, -144.6558853884952214 ) ) ;
#1952 = CIRCLE ( 'NONE', #11230, 7.500000000000007994 ) ;
#1953 = CARTESIAN_POINT ( 'NONE',  ( -380.0196196571620817, 63.47433729084224296, -117.1214152238070341 ) ) ;
#1954 = VERTEX_POINT ( 'NONE', #926 ) ;
#1955 = VECTOR ( 'NONE', #11204, 1000.000000000000000 ) ;
#1956 = CARTESIAN_POINT ( 'NONE',  ( -820.9141234758953942, 82.74039896267167649, -144.6672699209827613 ) ) ;
#1957 = CARTESIAN_POINT ( 'NONE',  ( -371.8698477746299886, 102.7100032247106469, -106.2096734411371557 ) ) ;
#1958 = DIRECTION ( 'NONE',  ( 1.000000000000000000, 0.000000000000000000, 0.000000000000000000 ) ) ;
#1959 = EDGE_LOOP ( 'NONE', ( #10356, #3461, #11148, #3797, #7547, #7980 ) ) ;
#1960 = CARTESIAN_POINT ( 'NONE',  ( -817.7441816825951264, 35.12288937987695903, -107.9061927053327281 ) ) ;
#1961 = CARTESIAN_POINT ( 'NONE',  ( 0.000000000000000000, -6.000000000000000000, -126.4213562373094959 ) ) ;
#1962 = CARTESIAN_POINT ( 'NONE',  ( 6.899999999999999467, 8.999999999999998224, 0.000000000000000000 ) ) ;
#1963 = DIRECTION ( 'NONE',  ( 0.000000000000000000, 0.000000000000000000, -1.000000000000000000 ) ) ;
#1964 = DIRECTION ( 'NONE',  ( 0.000000000000000000, 1.000000000000000000, 0.000000000000000000 ) ) ;
#1965 = AXIS2_PLACEMENT_3D ( 'NONE', #11493, #7661, #5795 ) ;
#1966 = PRODUCT_DEFINITION_CONTEXT ( 'detailed design', #7796, 'design' ) ;
#1967 = DIRECTION ( 'NONE',  ( 0.000000000000000000, 0.000000000000000000, -1.000000000000000000 ) ) ;
#1968 = AXIS2_PLACEMENT_3D ( 'NONE', #7539, #11492, #6671 ) ;
#1969 = VERTEX_POINT ( 'NONE', #3753 ) ;
#1970 = CARTESIAN_POINT ( 'NONE',  ( 9.184850993605165694E-16, -494.9999999999998863, -133.9213562373095101 ) ) ;
#1971 = CARTESIAN_POINT ( 'NONE',  ( -374.2661435795450871, 93.45316928466465356, -108.1938755228533182 ) ) ;
#1972 = AXIS2_PLACEMENT_3D ( 'NONE', #1669, #2530, #11129 ) ;
#1973 = CLOSED_SHELL ( 'NONE', ( #1030, #2315, #10373, #8644, #12238, #11825, #10263, #3894, #704, #12063, #5255, #9325 ) ) ;
#1974 = ORIENTED_EDGE ( 'NONE', *, *, #4514, .T. ) ;
#1975 = CARTESIAN_POINT ( 'NONE',  ( -954.5323978148114747, 113.6695689568732206, -103.3307627799632513 ) ) ;
#1976 = CARTESIAN_POINT ( 'NONE',  ( 0.000000000000000000, 12.00000000000000000, -89.68077099980401101 ) ) ;
#1977 = FACE_OUTER_BOUND ( 'NONE', #4833, .T. ) ;
#1978 = CARTESIAN_POINT ( 'NONE',  ( 20.96631641705466365, 181.6890404706723530, -124.5993264551280646 ) ) ;
#1979 = CARTESIAN_POINT ( 'NONE',  ( -1037.337636019038655, 116.9882293220588991, -122.7172756069792001 ) ) ;
#1980 = ORIENTED_EDGE ( 'NONE', *, *, #1201, .F. ) ;
#1981 = DIRECTION ( 'NONE',  ( 0.000000000000000000, 1.000000000000000000, -0.000000000000000000 ) ) ;
#1982 = DIRECTION ( 'NONE',  ( 0.000000000000000000, -0.000000000000000000, -1.000000000000000000 ) ) ;
#1983 = CARTESIAN_POINT ( 'NONE',  ( -1018.154501869017849, 114.3413228342528214, -141.4553492942762887 ) ) ;
#1984 = EDGE_CURVE ( 'NONE', #6153, #6536, #4698, .T. ) ;
#1985 = DIRECTION ( 'NONE',  ( 0.000000000000000000, 1.000000000000000000, 0.000000000000000000 ) ) ;
#1986 = LINE ( 'NONE', #1063, #10737 ) ;
#1987 = DIRECTION ( 'NONE',  ( 3.061276722312011504E-17, -1.000000000000000000, -0.000000000000000000 ) ) ;
#1988 = VERTEX_POINT ( 'NONE', #8472 ) ;
#1989 = CARTESIAN_POINT ( 'NONE',  ( -926.8105964072267398, 116.1567348237267083, -146.0307792196442733 ) ) ;
#1990 = CARTESIAN_POINT ( 'NONE',  ( 7.500000000000008882, 152.0000000000000000, -126.4213562373094959 ) ) ;
#1991 = ORIENTED_EDGE ( 'NONE', *, *, #2465, .T. ) ;
#1992 = ORIENTED_EDGE ( 'NONE', *, *, #8592, .T. ) ;
#1993 = CARTESIAN_POINT ( 'NONE',  ( 20.76787417662263735, 179.4594239414511492, -123.5091856982008949 ) ) ;
#1994 = DIRECTION ( 'NONE',  ( 0.000000000000000000, 0.000000000000000000, 1.000000000000000000 ) ) ;
#1995 = CARTESIAN_POINT ( 'NONE',  ( -20.00032812729986631, 181.6954111208232518, -124.4177824055624058 ) ) ;
#1996 = CARTESIAN_POINT ( 'NONE',  ( -927.9936929689694125, 74.21188826700395680, -149.7857175106638863 ) ) ;
#1997 = ORIENTED_EDGE ( 'NONE', *, *, #898, .F. ) ;
#1998 = EDGE_CURVE ( 'NONE', #5359, #6447, #5782, .T. ) ;
#1999 = CARTESIAN_POINT ( 'NONE',  ( -374.9802614396505760, 80.28172288411161617, -154.6205875143999435 ) ) ;
#2000 = DIRECTION ( 'NONE',  ( 0.000000000000000000, 0.000000000000000000, -1.000000000000000000 ) ) ;
#2001 = CARTESIAN_POINT ( 'NONE',  ( -382.7837046478651928, 69.53043186086833316, -109.0405781650321018 ) ) ;
#2002 = ADVANCED_FACE ( 'NONE', ( #11048 ), #7528, .F. ) ;
#2003 = CARTESIAN_POINT ( 'NONE',  ( 35.00000000000000000, 81.99999999999998579, 190.3192290001959748 ) ) ;
#2004 = CARTESIAN_POINT ( 'NONE',  ( -1065.000000000007049, 54.10491585757074517, -136.2353035311986389 ) ) ;
#2005 = ORIENTED_EDGE ( 'NONE', *, *, #3262, .F. ) ;
#2006 = PRODUCT ( 'MAS-313', 'MAS-313', '', ( #8566 ) ) ;
#2007 = CARTESIAN_POINT ( 'NONE',  ( 1.562900236585165577E-12, 12.00000000000000000, 16.07864376269049700 ) ) ;
#2008 = CARTESIAN_POINT ( 'NONE',  ( -956.2104666674714508, 71.56905446038054208, -96.78565065507946485 ) ) ;
#2009 = CARTESIAN_POINT ( 'NONE',  ( -827.6025323198989554, 81.97067649012242896, -104.6794282814521750 ) ) ;
#2010 = EDGE_LOOP ( 'NONE', ( #6975, #4556 ) ) ;
#2011 = CARTESIAN_POINT ( 'NONE',  ( -379.7921418149325063, 63.07164944986214294, -118.2218589047913611 ) ) ;
#2012 = CARTESIAN_POINT ( 'NONE',  ( -1011.051362836436624, 118.1813008219153716, -136.2353035311982126 ) ) ;
#2013 = ORIENTED_EDGE ( 'NONE', *, *, #6969, .F. ) ;
#2014 =( NAMED_UNIT ( * ) PLANE_ANGLE_UNIT ( ) SI_UNIT ( $, .RADIAN. ) );
#2015 = VERTEX_POINT ( 'NONE', #9322 ) ;
#2016 = AXIS2_PLACEMENT_3D ( 'NONE', #1419, #8941, #476 ) ;
#2017 = CARTESIAN_POINT ( 'NONE',  ( -795.0000000000039790, 60.65002596136936575, -103.3307627799632797 ) ) ;
#2018 = EDGE_CURVE ( 'NONE', #3679, #10836, #2419, .T. ) ;
#2019 = DIRECTION ( 'NONE',  ( -8.163404592832030268E-17, 1.000000000000000000, -0.000000000000000000 ) ) ;
#2020 = PLANE ( 'NONE',  #8399 ) ;
#2021 = EDGE_CURVE ( 'NONE', #4400, #6830, #5349, .T. ) ;
#2022 = CARTESIAN_POINT ( 'NONE',  ( -21.06555081338637692, 179.0416688902717510, -125.8654226178028068 ) ) ;
#2023 = CARTESIAN_POINT ( 'NONE',  ( 45.00000000000000711, 138.9999999999999716, -126.4213562373094959 ) ) ;
#2024 = CIRCLE ( 'NONE', #11878, 7.500000000000020428 ) ;
#2025 = ORIENTED_EDGE ( 'NONE', *, *, #8381, .F. ) ;
#2026 = CARTESIAN_POINT ( 'NONE',  ( 0.000000000000000000, 152.0000000000000000, -89.68077099980384048 ) ) ;
#2027 = ORIENTED_EDGE ( 'NONE', *, *, #8509, .F. ) ;
#2028 = CARTESIAN_POINT ( 'NONE',  ( -1014.007272717921069, 117.9006809476441049, -113.1262384684097526 ) ) ;
#2029 = EDGE_CURVE ( 'NONE', #6191, #2820, #8606, .T. ) ;
#2030 = DIRECTION ( 'NONE',  ( 0.000000000000000000, 1.000000000000000000, 0.000000000000000000 ) ) ;
#2031 = AXIS2_PLACEMENT_3D ( 'NONE', #6574, #2608, #7434 ) ;
#2032 = SHAPE_REPRESENTATION ( 'Base Mount Flange', ( #11957 ), #5231 ) ;
#2033 = CARTESIAN_POINT ( 'NONE',  ( 3.133148353965215262E-13, -6.000000000000004441, -103.9213562373094959 ) ) ;
#2034 = EDGE_LOOP ( 'NONE', ( #2196, #8986 ) ) ;
#2035 = DIRECTION ( 'NONE',  ( 0.000000000000000000, 1.000000000000000000, 0.000000000000000000 ) ) ;
#2036 = CARTESIAN_POINT ( 'NONE',  ( -818.8285638327206470, 78.67432280806531253, -104.9592124606049879 ) ) ;
#2037 = FACE_BOUND ( 'NONE', #3887, .T. ) ;
#2038 = CARTESIAN_POINT ( 'NONE',  ( -974.6181169426273527, 104.3135445892218200, -149.7857175106634884 ) ) ;
#2039 = FILL_AREA_STYLE_COLOUR ( '', #5518 ) ;
#2040 = CARTESIAN_POINT ( 'NONE',  ( 35.00000000000000000, 163.9999999999999716, 190.3192290001959748 ) ) ;
#2041 = LINE ( 'NONE', #11434, #11152 ) ;
#2042 = VERTEX_POINT ( 'NONE', #2026 ) ;
#2043 = LINE ( 'NONE', #8874, #9637 ) ;
#2044 = CARTESIAN_POINT ( 'NONE',  ( -1031.197907781699314, 107.2697845108579173, -146.0307792196445291 ) ) ;
#2045 = CIRCLE ( 'NONE', #10527, 7.500000000000007105 ) ;
#2046 = PLANE ( 'NONE',  #629 ) ;
#2047 = EDGE_LOOP ( 'NONE', ( #3070, #10949 ) ) ;
#2048 = EDGE_LOOP ( 'NONE', ( #3175, #9799 ) ) ;
#2049 = CARTESIAN_POINT ( 'NONE',  ( 20.85245725203401079, 179.0178972154230621, -123.9104686020650519 ) ) ;
#2050 = DIRECTION ( 'NONE',  ( -0.000000000000000000, 0.5000000000000009992, 0.8660254037844380415 ) ) ;
#2051 = CARTESIAN_POINT ( 'NONE',  ( -819.8422515189698743, 75.63891865958764527, -105.7172146583293681 ) ) ;
#2052 = FACE_BOUND ( 'NONE', #6778, .T. ) ;
#2053 = CARTESIAN_POINT ( 'NONE',  ( -1016.652307257396728, 63.31440937415337800, -146.0307792196454102 ) ) ;
#2054 = CIRCLE ( 'NONE', #12131, 7.500000000000013323 ) ;
#2055 = VERTEX_POINT ( 'NONE', #10429 ) ;
#2056 = CIRCLE ( 'NONE', #8389, 7.500000000000007105 ) ;
#2057 = CARTESIAN_POINT ( 'NONE',  ( -373.8927214104571135, 69.57595966422515232, -151.1258107129636699 ) ) ;
#2058 = CARTESIAN_POINT ( 'NONE',  ( -30.53136272649514638, 180.2041921146316668, -134.6807709998038547 ) ) ;
#2059 = CARTESIAN_POINT ( 'NONE',  ( -383.2380640590296252, 70.81816280502410166, -108.0477105264665880 ) ) ;
#2060 = DIRECTION ( 'NONE',  ( 0.7071067811865473507, 0.000000000000000000, -0.7071067811865477948 ) ) ;
#2061 = VERTEX_POINT ( 'NONE', #1970 ) ;
#2062 = CARTESIAN_POINT ( 'NONE',  ( -954.5446161821218993, 49.54000128949421367, -130.5712005305404091 ) ) ;
#2063 = CIRCLE ( 'NONE', #672, 7.500000000000007105 ) ;
#2064 = VERTEX_POINT ( 'NONE', #10365 ) ;
#2065 = EDGE_CURVE ( 'NONE', #5919, #11269, #7707, .T. ) ;
#2066 = AXIS2_PLACEMENT_3D ( 'NONE', #10321, #3831, #9518 ) ;
#2067 = VECTOR ( 'NONE', #10887, 1000.000000000000000 ) ;
#2068 = DIRECTION ( 'NONE',  ( -1.000000000000000000, 0.000000000000000000, 0.000000000000000000 ) ) ;
#2069 = EDGE_CURVE ( 'NONE', #10717, #3207, #440, .T. ) ;
#2070 = CARTESIAN_POINT ( 'NONE',  ( -975.7625022073081027, 55.15120678236761620, -99.57582448894500260 ) ) ;
#2071 = DIRECTION ( 'NONE',  ( 0.000000000000000000, 0.000000000000000000, 1.000000000000000000 ) ) ;
#2072 = CARTESIAN_POINT ( 'NONE',  ( -1065.000000000007049, 54.10491585757074517, -136.2353035311986389 ) ) ;
#2073 = VERTEX_POINT ( 'NONE', #11418 ) ;
#2074 = CARTESIAN_POINT ( 'NONE',  ( -818.8285638327238303, 78.67432280806571043, -144.4023295390032899 ) ) ;
#2075 = CARTESIAN_POINT ( 'NONE',  ( -384.1464637028664697, 74.21013607762992592, -106.2506866248873365 ) ) ;
#2076 = VERTEX_POINT ( 'NONE', #2094 ) ;
#2077 = CARTESIAN_POINT ( 'NONE',  ( 1.479627290717497352E-14, 152.0000000000000284, 118.9213562373094817 ) ) ;
#2078 = VERTEX_POINT ( 'NONE', #5728 ) ;
#2079 = EDGE_CURVE ( 'NONE', #7375, #11612, #2045, .T. ) ;
#2080 = AXIS2_PLACEMENT_3D ( 'NONE', #6022, #262, #4051 ) ;
#2081 = DIRECTION ( 'NONE',  ( 0.000000000000000000, 0.000000000000000000, 1.000000000000000000 ) ) ;
#2082 = CIRCLE ( 'NONE', #3440, 7.500000000000013323 ) ;
#2083 = ORIENTED_EDGE ( 'NONE', *, *, #9085, .T. ) ;
#2084 = CARTESIAN_POINT ( 'NONE',  ( -1065.000000000004093, 52.00000000000021316, -122.7172756069792854 ) ) ;
#2085 = DIRECTION ( 'NONE',  ( -8.163404592832030268E-17, 1.000000000000000000, -0.000000000000000000 ) ) ;
#2086 = DIRECTION ( 'NONE',  ( -8.163404592832030268E-17, 1.000000000000000000, -0.000000000000000000 ) ) ;
#2087 = PRODUCT_DEFINITION_CONTEXT ( 'detailed design', #6531, 'design' ) ;
#2088 = VECTOR ( 'NONE', #6452, 1000.000000000000000 ) ;
#2089 = AXIS2_PLACEMENT_3D ( 'NONE', #10446, #1987, #6861 ) ;
#2090 = DIRECTION ( 'NONE',  ( 0.000000000000000000, 0.000000000000000000, 1.000000000000000000 ) ) ;
#2091 = CARTESIAN_POINT ( 'NONE',  ( -21.06800052547805535, 179.2509983577178616, -126.0809827838107964 ) ) ;
#2092 = ADVANCED_FACE ( 'NONE', ( #4806 ), #8702, .F. ) ;
#2093 = VERTEX_POINT ( 'NONE', #1221 ) ;
#2094 = CARTESIAN_POINT ( 'NONE',  ( 3.123963502971610252E-13, 12.00000000000000000, -88.92135623730948168 ) ) ;
#2095 = ORIENTED_EDGE ( 'NONE', *, *, #5571, .F. ) ;
#2096 = CARTESIAN_POINT ( 'NONE',  ( -1065.000000000005230, 87.89043812168627312, -95.06748246948058068 ) ) ;
#2097 = PRODUCT_RELATED_PRODUCT_CATEGORY ( 'part', '', ( #2006 ) ) ;
#2098 = CARTESIAN_POINT ( 'NONE',  ( -1013.901471336339000, 119.8325901201404804, -130.5712005305404944 ) ) ;
#2099 = FACE_OUTER_BOUND ( 'NONE', #7879, .T. ) ;
#2100 = ORIENTED_EDGE ( 'NONE', *, *, #3197, .T. ) ;
#2101 = CARTESIAN_POINT ( 'NONE',  ( 1.875296586882326249E-12, 152.0000000000000000, 46.07864376269051121 ) ) ;
#2102 = EDGE_CURVE ( 'NONE', #10282, #8579, #884, .T. ) ;
#2103 = CARTESIAN_POINT ( 'NONE',  ( 1.142876642996484321E-14, 24.00000000000001421, -126.4213562373094959 ) ) ;
#2104 = CARTESIAN_POINT ( 'NONE',  ( -150.0000000000000000, -9.213203435596451385, -126.4213562373084301 ) ) ;
#2105 = FACE_OUTER_BOUND ( 'NONE', #1033, .T. ) ;
#2106 = CARTESIAN_POINT ( 'NONE',  ( -1045.967528061855091, 112.8272211019271225, -136.2353035311980705 ) ) ;
#2107 = CARTESIAN_POINT ( 'NONE',  ( 9.184850993605149917E-16, -6.000000000000000000, -133.9213562373095101 ) ) ;
#2108 = ORIENTED_EDGE ( 'NONE', *, *, #542, .T. ) ;
#2109 = DIRECTION ( 'NONE',  ( 0.000000000000000000, -1.000000000000000000, -7.930164461608263644E-17 ) ) ;
#2110 = CARTESIAN_POINT ( 'NONE',  ( -822.2439855206093853, 97.57287547056431265, -149.7857175106634600 ) ) ;
#2111 = FACE_BOUND ( 'NONE', #9135, .T. ) ;
#2112 = ORIENTED_EDGE ( 'NONE', *, *, #1121, .F. ) ;
#2113 = VECTOR ( 'NONE', #908, 1000.000000000000000 ) ;
#2114 = ORIENTED_EDGE ( 'NONE', *, *, #414, .F. ) ;
#2115 = CARTESIAN_POINT ( 'NONE',  ( -381.8407521777220950, 96.85938717894678973, -138.1176283752880067 ) ) ;
#2116 = DIRECTION ( 'NONE',  ( 0.000000000000000000, 0.000000000000000000, 1.000000000000000000 ) ) ;
#2117 = CARTESIAN_POINT ( 'NONE',  ( -1020.430183747032629, 74.13649791779326392, -152.5758913445297651 ) ) ;
#2118 = ORIENTED_EDGE ( 'NONE', *, *, #12020, .T. ) ;
#2119 = CARTESIAN_POINT ( 'NONE',  ( -374.9887786383590651, 80.39322394422208617, -144.6212526005259065 ) ) ;
#2120 = CARTESIAN_POINT ( 'NONE',  ( -126.4213562373094959, -494.9999999999998863, 2.255140518769849223E-14 ) ) ;
#2121 = CARTESIAN_POINT ( 'NONE',  ( -374.9884691243568113, 80.37146653597520185, -104.7419479422377577 ) ) ;
#2122 = VECTOR ( 'NONE', #2385, 999.9999999999998863 ) ;
#2123 = CARTESIAN_POINT ( 'NONE',  ( -270.0000000000000000, 24.00000000000000711, -126.4213562373076059 ) ) ;
#2124 = DIRECTION ( 'NONE',  ( 0.000000000000000000, 0.000000000000000000, -1.000000000000000000 ) ) ;
#2125 = ORIENTED_EDGE ( 'NONE', *, *, #6530, .F. ) ;
#2126 = EDGE_LOOP ( 'NONE', ( #1513, #11428, #1925, #8252 ) ) ;
#2127 = CIRCLE ( 'NONE', #8642, 7.500000000000007105 ) ;
#2128 = CARTESIAN_POINT ( 'NONE',  ( 6.247927005943220505E-13, -6.000000000000006217, -58.92135623730948879 ) ) ;
#2129 = CARTESIAN_POINT ( 'NONE',  ( 21.01976670805043312, 178.7020268087202055, -125.0612880804587093 ) ) ;
#2130 = AXIS2_PLACEMENT_3D ( 'NONE', #11448, #8548, #1136 ) ;
#2131 = CARTESIAN_POINT ( 'NONE',  ( -997.7839878466058963, 40.27522178589197921, -113.1262384684093547 ) ) ;
#2132 = CARTESIAN_POINT ( 'NONE',  ( -822.5306970061956235, 83.50573423571573528, -104.7374748144106462 ) ) ;
#2133 = ORIENTED_EDGE ( 'NONE', *, *, #4354, .T. ) ;
#2134 = CARTESIAN_POINT ( 'NONE',  ( -818.8285638327239440, 79.00056486032038094, -144.4573442453753103 ) ) ;
#2135 = CARTESIAN_POINT ( 'NONE',  ( -384.9561085268001648, 84.12206627636906831, -104.7580990804535759 ) ) ;
#2136 = CARTESIAN_POINT ( 'NONE',  ( 141.4213562373095101, 0.000000000000000000, -1.508194112741312283E-14 ) ) ;
#2137 = EDGE_LOOP ( 'NONE', ( #5105, #4327, #5467, #4968 ) ) ;
#2138 = ADVANCED_FACE ( 'NONE', ( #9503 ), #8580, .F. ) ;
#2139 = VERTEX_POINT ( 'NONE', #1904 ) ;
#2140 = CARTESIAN_POINT ( 'NONE',  ( -1021.637154595298057, 53.81063926482157456, -122.7172756069792285 ) ) ;
#2141 = VECTOR ( 'NONE', #2060, 999.9999999999998863 ) ;
#2142 = CYLINDRICAL_SURFACE ( 'NONE', #5804, 7.500000000000007105 ) ;
#2143 = VECTOR ( 'NONE', #5403, 1000.000000000000000 ) ;
#2144 = CARTESIAN_POINT ( 'NONE',  ( -853.0139081111171890, 107.1087209265617020, -103.3307627799635355 ) ) ;
#2145 = LINE ( 'NONE', #2894, #10261 ) ;
#2146 = CARTESIAN_POINT ( 'NONE',  ( -19.98209572305366422, 179.3222604960775186, -125.8830796407651036 ) ) ;
#2147 = CIRCLE ( 'NONE', #9240, 7.500000000000020428 ) ;
#2148 = ORIENTED_EDGE ( 'NONE', *, *, #8496, .F. ) ;
#2149 = DIRECTION ( 'NONE',  ( 0.000000000000000000, 0.000000000000000000, -1.000000000000000000 ) ) ;
#2150 = ORIENTED_EDGE ( 'NONE', *, *, #5872, .F. ) ;
#2152 = ADVANCED_FACE ( 'NONE', ( #5669 ), #9445, .F. ) ;
#2151 = CARTESIAN_POINT ( 'NONE',  ( -1061.276350651669873, 98.40484402385480678, -99.57582448894525839 ) ) ;
#2153 = AXIS2_PLACEMENT_3D ( 'NONE', #228, #994, #1982 ) ;
#2154 = ORIENTED_EDGE ( 'NONE', *, *, #793, .F. ) ;
#2155 = CARTESIAN_POINT ( 'NONE',  ( -1014.007272717915953, 117.9006809476442896, -136.2353035311982126 ) ) ;
#2156 = CARTESIAN_POINT ( 'NONE',  ( 19.00000000000000355, 168.0000000000000000, -124.6807709998038405 ) ) ;
#2157 = VECTOR ( 'NONE', #11936, 1000.000000000000000 ) ;
#2158 = DIRECTION ( 'NONE',  ( -1.000000000000000000, -0.000000000000000000, 0.000000000000000000 ) ) ;
#2159 = CARTESIAN_POINT ( 'NONE',  ( -1010.922847972426780, 120.6260792194948550, -122.7172756069790296 ) ) ;
#2160 = ORIENTED_EDGE ( 'NONE', *, *, #2605, .T. ) ;
#2161 = DIRECTION ( 'NONE',  ( 0.000000000000000000, 0.000000000000000000, 1.000000000000000000 ) ) ;
#2162 =( GEOMETRIC_REPRESENTATION_CONTEXT ( 3 ) GLOBAL_UNCERTAINTY_ASSIGNED_CONTEXT ( ( #8812 ) ) GLOBAL_UNIT_ASSIGNED_CONTEXT ( ( #2722, #12126, #6304 ) ) REPRESENTATION_CONTEXT ( 'NONE', 'WORKASPACE' ) );
#2163 = DIRECTION ( 'NONE',  ( 0.000000000000000000, 1.000000000000000000, 0.000000000000000000 ) ) ;
#2164 = LINE ( 'NONE', #9694, #10636 ) ;
#2165 = CLOSED_SHELL ( 'NONE', ( #4044, #4135, #1107, #10753, #9538, #7591, #8135, #6025, #5853, #8512, #8603, #6024, #5151, #5797, #10679, #10361, #11136, #7834, #1408, #7906, #4103, #8920, #9107, #11510, #1630, #8821, #4879, #2972, #3912, #10785, #11835, #5452, #478, #9270, #5298, #10516, #22, #2152, #11139, #2444, #6303, #11118, #1277, #5788, #3667, #11622, #5767, #8124, #11426, #2822, #9473, #7376, #11174, #12222, #6697, #7422, #553, #12229, #270 ) ) ;
#2166 = CARTESIAN_POINT ( 'NONE',  ( -1017.963927524549604, 117.4283576114808625, -136.2353035311979284 ) ) ;
#2167 = DIRECTION ( 'NONE',  ( -0.9501779778103371932, 0.000000000000000000, 0.3117078928809124960 ) ) ;
#2168 = CARTESIAN_POINT ( 'NONE',  ( -210.0000000000000000, 151.9999999999999716, -126.4213562373080180 ) ) ;
#2169 = CARTESIAN_POINT ( 'NONE',  ( -29.99999999999998934, 24.00000000000001421, -126.4213562373092685 ) ) ;
#2170 = VERTEX_POINT ( 'NONE', #11608 ) ;
#2171 = CARTESIAN_POINT ( 'NONE',  ( -1010.922847972425529, 120.6260792194948550, -124.6807709998039542 ) ) ;
#2172 = EDGE_CURVE ( 'NONE', #10880, #11915, #3222, .T. ) ;
#2173 = VECTOR ( 'NONE', #8279, 1000.000000000000000 ) ;
#2174 = LINE ( 'NONE', #5937, #7546 ) ;
#2175 = ORIENTED_EDGE ( 'NONE', *, *, #11470, .F. ) ;
#2176 = ORIENTED_EDGE ( 'NONE', *, *, #8867, .T. ) ;
#2177 = EDGE_CURVE ( 'NONE', #10646, #7797, #339, .T. ) ;
#2178 = CARTESIAN_POINT ( 'NONE',  ( -380.2702075887810906, 100.0761580381868896, -133.3173879207189998 ) ) ;
#2179 = CARTESIAN_POINT ( 'NONE',  ( -975.7625022073049195, 55.15120678236734619, -149.7857175106636589 ) ) ;
#2180 = CARTESIAN_POINT ( 'NONE',  ( -819.0908526083459265, 77.06787236046235989, -144.0637517540457679 ) ) ;
#2181 = CARTESIAN_POINT ( 'NONE',  ( -27.10787553788296833, 180.2041921146317236, -137.3302880892916846 ) ) ;
#2182 = CARTESIAN_POINT ( 'NONE',  ( 6.899999999999999467, 8.999999999999998224, 0.000000000000000000 ) ) ;
#2183 = CARTESIAN_POINT ( 'NONE',  ( 0.000000000000000000, -7.794228634059935601, 4.500000000000016875 ) ) ;
#2184 = CARTESIAN_POINT ( 'NONE',  ( -151.3258811035894098, 12.00000000000000000, -56.13263083939680342 ) ) ;
#2185 = ADVANCED_FACE ( 'NONE', ( #1448 ), #10920, .T. ) ;
#2186 = EDGE_LOOP ( 'NONE', ( #4571, #11548, #991, #8312 ) ) ;
#2187 = ORIENTED_EDGE ( 'NONE', *, *, #4356, .F. ) ;
#2188 = CARTESIAN_POINT ( 'NONE',  ( -817.7441816825951264, 35.12288937987695903, -107.9061927053327281 ) ) ;
#2189 = CARTESIAN_POINT ( 'NONE',  ( -19.84927175247429432, 181.0689383095263167, -127.1322084511289034 ) ) ;
#2190 = CARTESIAN_POINT ( 'NONE',  ( -202.4999999999999716, 139.9999999999999716, -126.4213562373080180 ) ) ;
#2191 = CARTESIAN_POINT ( 'NONE',  ( -380.7160366723977063, 64.77876409789038803, -114.4938704800854907 ) ) ;
#2192 = EDGE_LOOP ( 'NONE', ( #1719, #9089 ) ) ;
#2193 = CARTESIAN_POINT ( 'NONE',  ( -262.5000000000000000, 151.9999999999999716, -126.4213562373076059 ) ) ;
#2194 = VERTEX_POINT ( 'NONE', #10728 ) ;
#2195 = CONTEXT_DEPENDENT_SHAPE_REPRESENTATION ( #3765, #9602 ) ;
#2196 = ORIENTED_EDGE ( 'NONE', *, *, #4570, .F. ) ;
#2197 = CARTESIAN_POINT ( 'NONE',  ( -928.4368846968627622, 59.55532739646334051, -122.7172756069790154 ) ) ;
#2198 = DIRECTION ( 'NONE',  ( -0.000000000000000000, 1.000000000000000000, -0.000000000000000000 ) ) ;
#2199 = DIRECTION ( 'NONE',  ( 0.000000000000000000, 0.000000000000000000, 1.000000000000000000 ) ) ;
#2200 = CIRCLE ( 'NONE', #611, 15.52076803445812203 ) ;
#2201 = CARTESIAN_POINT ( 'NONE',  ( -1011.662592067698938, 105.4443429699071828, -99.57582448894505944 ) ) ;
#2202 = CARTESIAN_POINT ( 'NONE',  ( 21.06714545844871367, 179.4370239411119030, -126.2109676220344596 ) ) ;
#2203 = ORIENTED_EDGE ( 'NONE', *, *, #11459, .T. ) ;
#2204 = CARTESIAN_POINT ( 'NONE',  ( 2.498657532616778856E-14, -6.999999999999978684, -124.6807709998038405 ) ) ;
#2205 = ORIENTED_EDGE ( 'NONE', *, *, #944, .T. ) ;
#2206 = CARTESIAN_POINT ( 'NONE',  ( -927.1204550305436669, 105.3607176047075029, -96.78565065507918064 ) ) ;
#2207 = ORIENTED_EDGE ( 'NONE', *, *, #9846, .F. ) ;
#2208 = CARTESIAN_POINT ( 'NONE',  ( -904.1919162299276422, 124.8346192645298487, -130.5712005305403807 ) ) ;
#2209 = DIRECTION ( 'NONE',  ( 0.000000000000000000, 0.5000000000000009992, -0.8660254037844380415 ) ) ;
#2210 = CARTESIAN_POINT ( 'NONE',  ( 1.875296586882326249E-12, -6.000000000000004441, 46.07864376269049700 ) ) ;
#2211 = AXIS2_PLACEMENT_3D ( 'NONE', #3083, #8829, #4817 ) ;
#2212 = CIRCLE ( 'NONE', #11498, 7.500000000000013323 ) ;
#2213 = ADVANCED_FACE ( 'NONE', ( #8984 ), #1394, .F. ) ;
#2214 = VERTEX_POINT ( 'NONE', #3354 ) ;
#2215 = EDGE_CURVE ( 'NONE', #8134, #10520, #2245, .T. ) ;
#2216 = CARTESIAN_POINT ( 'NONE',  ( -822.6918648528270523, 83.54617135775964698, -104.7406007859484873 ) ) ;
#2217 = DIRECTION ( 'NONE',  ( 0.000000000000000000, 1.000000000000000000, 0.000000000000000000 ) ) ;
#2218 = CARTESIAN_POINT ( 'NONE',  ( 21.06714545844871367, 179.4370239411119030, -126.2109676220344596 ) ) ;
#2219 = DIRECTION ( 'NONE',  ( 0.000000000000000000, 1.000000000000000000, 0.000000000000000000 ) ) ;
#2220 = ORIENTED_EDGE ( 'NONE', *, *, #12118, .F. ) ;
#2221 = CARTESIAN_POINT ( 'NONE',  ( -305.0000000000000568, 81.99999999999995737, -89.68077099980384048 ) ) ;
#2222 = AXIS2_PLACEMENT_3D ( 'NONE', #11831, #3287, #8906 ) ;
#2223 = ADVANCED_FACE ( 'NONE', ( #7138 ), #5158, .F. ) ;
#2224 = DIRECTION ( 'NONE',  ( -0.000000000000000000, 1.000000000000000000, 7.930164461608263644E-17 ) ) ;
#2225 = CARTESIAN_POINT ( 'NONE',  ( -954.3284336448712111, 118.5422944683825932, -141.4553492942762318 ) ) ;
#2226 = DIRECTION ( 'NONE',  ( 0.000000000000000000, 1.000000000000000000, 0.000000000000000000 ) ) ;
#2227 = LINE ( 'NONE', #11634, #3383 ) ;
#2228 = ORIENTED_EDGE ( 'NONE', *, *, #9358, .F. ) ;
#2229 = ORIENTED_EDGE ( 'NONE', *, *, #8271, .F. ) ;
#2230 = AXIS2_PLACEMENT_3D ( 'NONE', #12204, #3728, #7 ) ;
#2231 = EDGE_CURVE ( 'NONE', #10646, #9219, #7977, .T. ) ;
#2232 = CARTESIAN_POINT ( 'NONE',  ( -823.1660337641055776, 73.70728137675567382, -106.4808805636502740 ) ) ;
#2233 = CARTESIAN_POINT ( 'NONE',  ( -1025.323167507848893, 62.35287014669186334, -146.0307792196450691 ) ) ;
#2234 = CYLINDRICAL_SURFACE ( 'NONE', #9598, 5.000000000000115463 ) ;
#2235 = ADVANCED_FACE ( 'NONE', ( #5972 ), #1285, .F. ) ;
#2236 = DIRECTION ( 'NONE',  ( 1.000000000000000000, 0.000000000000000000, 0.000000000000000000 ) ) ;
#2237 = DIRECTION ( 'NONE',  ( -1.000000000000000000, 0.000000000000000000, 0.000000000000000000 ) ) ;
#2238 = B_SPLINE_CURVE_WITH_KNOTS ( 'NONE', 3,
 ( #4308, #3360, #453, #8079, #3483, #11901, #11848, #6224, #6279, #5279, #9054, #592, #4366, #8269, #3419, #4429, #2329, #12027, #7208, #2502, #10049, #8205, #11964, #11035, #2564, #10108, #7021, #1399, #10389, #1571, #7385, #6269, #11956, #5392, #6391, #1696 ),
 .UNSPECIFIED., .F., .F.,
 ( 4, 2, 2, 2, 2, 2, 2, 2, 2, 2, 2, 2, 2, 2, 2, 2, 2, 4 ),
 ( 0.01563545586487890063, 0.01661450767168204737, 0.01759355947848519064, 0.01857261128528833738, 0.01955166309209148412, 0.02053071489889463086, 0.02150976670569777413, 0.02248881851250092087, 0.02346787031930406414, 0.02444692212610721088, 0.02493644802950895079, 0.02542597393291068722, 0.02640502573971446193, 0.02738407754651823664, 0.02836312935332201135, 0.02934218116012578953, 0.03032123296692956424, 0.03130028477373333895 ),
 .UNSPECIFIED. ) ;
#2239 = CARTESIAN_POINT ( 'NONE',  ( -828.5735791249488784, 77.06472017290390397, -94.70715242654415533 ) ) ;
#2240 = VECTOR ( 'NONE', #11289, 1000.000000000000000 ) ;
#2241 =( NAMED_UNIT ( * ) PLANE_ANGLE_UNIT ( ) SI_UNIT ( $, .RADIAN. ) );
#2242 = CARTESIAN_POINT ( 'NONE',  ( -997.9925905826634107, 37.72784750336339954, -130.5712005305403238 ) ) ;
#2243 = VECTOR ( 'NONE', #1586, 1000.000000000000000 ) ;
#2244 = EDGE_LOOP ( 'NONE', ( #4771, #7124 ) ) ;
#2245 = CIRCLE ( 'NONE', #4032, 7.500000000000007105 ) ;
#2246 = CARTESIAN_POINT ( 'NONE',  ( -1016.863910020555409, 59.13213530333446499, -107.9061927053325576 ) ) ;
#2247 = CARTESIAN_POINT ( 'NONE',  ( -30.00000000000000000, -492.9999999999998863, -30.00000000000000000 ) ) ;
#2248 = ORIENTED_EDGE ( 'NONE', *, *, #7195, .F. ) ;
#2249 = ADVANCED_FACE ( 'NONE', ( #10903 ), #7018, .T. ) ;
#2250 = CARTESIAN_POINT ( 'NONE',  ( 1.561981751485805177E-12, 12.00000000000000000, 23.57864376269050410 ) ) ;
#2251 = CARTESIAN_POINT ( 'NONE',  ( 126.4213562373094959, -492.9999999999998863, -6.938893903907228378E-15 ) ) ;
#2252 = ORIENTED_EDGE ( 'NONE', *, *, #3563, .F. ) ;
#2253 = CARTESIAN_POINT ( 'NONE',  ( -6.106226635438360972E-13, 12.00000000000000000, -244.6807709998039400 ) ) ;
#2254 = ORIENTED_EDGE ( 'NONE', *, *, #4322, .F. ) ;
#2255 = ORIENTED_EDGE ( 'NONE', *, *, #6451, .F. ) ;
#2256 = CARTESIAN_POINT ( 'NONE',  ( -1038.708781889661850, 41.03774456592562103, -118.7903414690682240 ) ) ;
#2257 = AXIS2_PLACEMENT_3D ( 'NONE', #1106, #1556, #5321 ) ;
#2258 = CIRCLE ( 'NONE', #5009, 7.500000000000012434 ) ;
#2259 = FACE_OUTER_BOUND ( 'NONE', #1365, .T. ) ;
#2260 = B_SPLINE_CURVE_WITH_KNOTS ( 'NONE', 3,
 ( #4171, #8188, #6030, #5204, #5266, #3349 ),
 .UNSPECIFIED., .F., .F.,
 ( 4, 2, 4 ),
 ( 0.008741033683305053648, 0.009157775081816015711, 0.009574516480326976040 ),
 .UNSPECIFIED. ) ;
#2261 = UNCERTAINTY_MEASURE_WITH_UNIT (LENGTH_MEASURE( 1.000000000000000082E-05 ), #7770, 'distance_accuracy_value', 'NONE');
#2262 = CARTESIAN_POINT ( 'NONE',  ( -1022.396981161626059, 109.5926079579672319, -103.3307627799638482 ) ) ;
#2263 = LINE ( 'NONE', #7896, #4761 ) ;
#2264 = CIRCLE ( 'NONE', #11341, 10.00000000000000355 ) ;
#2265 = ORIENTED_EDGE ( 'NONE', *, *, #7747, .F. ) ;
#2266 = CIRCLE ( 'NONE', #1464, 7.500000000000007105 ) ;
#2267 = EDGE_CURVE ( 'NONE', #3571, #7713, #9039, .T. ) ;
#2268 = VERTEX_POINT ( 'NONE', #7013 ) ;
#2269 = CARTESIAN_POINT ( 'NONE',  ( -853.1108559448483675, 99.60875591605646662, -99.57582448894477523 ) ) ;
#2270 = CARTESIAN_POINT ( 'NONE',  ( 19.98635603549800521, 182.5149518089054652, -123.9190205516158159 ) ) ;
#2271 = CARTESIAN_POINT ( 'NONE',  ( -954.0441199534431007, 124.9954171138389398, -126.6442663926288787 ) ) ;
#2272 = DIRECTION ( 'NONE',  ( 0.000000000000000000, 1.000000000000000000, -0.000000000000000000 ) ) ;
#2273 = CIRCLE ( 'NONE', #11162, 4.000000000000003553 ) ;
#2274 = FACE_OUTER_BOUND ( 'NONE', #11529, .T. ) ;
#2275 = AXIS2_PLACEMENT_3D ( 'NONE', #3443, #10192, #3500 ) ;
#2276 = CYLINDRICAL_SURFACE ( 'NONE', #8493, 7.500000000000007105 ) ;
#2277 = CARTESIAN_POINT ( 'NONE',  ( -45.53315400109751465, 0.000000000000000000, -237.8419396193594650 ) ) ;
#2278 = FACE_BOUND ( 'NONE', #8897, .T. ) ;
#2279 = CARTESIAN_POINT ( 'NONE',  ( 0.000000000000000000, 1.502314598737159426E-15, -9.000000000000000000 ) ) ;
#2280 = CARTESIAN_POINT ( 'NONE',  ( 20.99327390029534968, 178.6730123709782845, -124.7865744064447995 ) ) ;
#2281 = FACE_BOUND ( 'NONE', #9539, .T. ) ;
#2282 = VERTEX_POINT ( 'NONE', #8256 ) ;
#2283 = CYLINDRICAL_SURFACE ( 'NONE', #12150, 7.500000000000007105 ) ;
#2284 = DIRECTION ( 'NONE',  ( -1.000000000000000000, 0.000000000000000000, 0.000000000000000000 ) ) ;
#2285 = EDGE_CURVE ( 'NONE', #5774, #192, #3821, .T. ) ;
#2286 = EDGE_CURVE ( 'NONE', #694, #3418, #4234, .T. ) ;
#2287 = CARTESIAN_POINT ( 'NONE',  ( -19.03136272649511085, 180.2041921146316668, -134.6807709998038547 ) ) ;
#2288 = AXIS2_PLACEMENT_3D ( 'NONE', #5466, #9242, #3743 ) ;
#2289 = ORIENTED_EDGE ( 'NONE', *, *, #3136, .T. ) ;
#2290 = FACE_BOUND ( 'NONE', #6621, .T. ) ;
#2291 = CARTESIAN_POINT ( 'NONE',  ( -1026.651933061287082, 84.71212313386841686, -154.8742214401230228 ) ) ;
#2292 = CARTESIAN_POINT ( 'NONE',  ( -820.7495229154759500, 74.72132575352402739, -143.3103177350649844 ) ) ;
#2293 = CARTESIAN_POINT ( 'NONE',  ( 0.8038475772931109598, -5.196152422707023710, -9.000000000000001776 ) ) ;
#2294 = FACE_OUTER_BOUND ( 'NONE', #377, .T. ) ;
#2295 = CARTESIAN_POINT ( 'NONE',  ( -380.3383793650497751, 64.05796225469710237, -115.8204086816914611 ) ) ;
#2296 = LINE ( 'NONE', #4155, #967 ) ;
#2297 = DIRECTION ( 'NONE',  ( -0.000000000000000000, 1.000000000000000000, 7.930164461608263644E-17 ) ) ;
#2298 = ORIENTED_EDGE ( 'NONE', *, *, #8213, .T. ) ;
#2299 = EDGE_CURVE ( 'NONE', #5668, #7181, #7507, .T. ) ;
#2300 = CARTESIAN_POINT ( 'NONE',  ( 28.00000000000000000, -492.9999999999998863, -27.99999999999999645 ) ) ;
#2301 = CARTESIAN_POINT ( 'NONE',  ( -956.7203770923184720, 58.97922774997713447, -146.0307792196449839 ) ) ;
#2302 = EDGE_CURVE ( 'NONE', #6384, #5463, #8505, .T. ) ;
#2303 = VECTOR ( 'NONE', #12, 1000.000000000000000 ) ;
#2304 = ORIENTED_EDGE ( 'NONE', *, *, #11586, .T. ) ;
#2305 = ORIENTED_EDGE ( 'NONE', *, *, #4849, .F. ) ;
#2306 = ADVANCED_FACE ( 'NONE', ( #11334 ), #6639, .F. ) ;
#2307 = CARTESIAN_POINT ( 'NONE',  ( -1014.132585063772353, 52.13780504951625261, -122.7172756069792428 ) ) ;
#2308 = CARTESIAN_POINT ( 'NONE',  ( -19.96884611294068179, 180.9047917079184344, -123.3454246131005050 ) ) ;
#2309 = VERTEX_POINT ( 'NONE', #7442 ) ;
#2310 = AXIS2_PLACEMENT_3D ( 'NONE', #10161, #4546, #6327 ) ;
#2311 = LINE ( 'NONE', #6080, #8141 ) ;
#2312 = CARTESIAN_POINT ( 'NONE',  ( -823.1766404291720391, 73.70610174456017205, -154.6458666179561590 ) ) ;
#2313 = ORIENTED_EDGE ( 'NONE', *, *, #4480, .F. ) ;
#2314 = ORIENTED_EDGE ( 'NONE', *, *, #7359, .F. ) ;
#2315 = ADVANCED_FACE ( 'NONE', ( #11225 ), #10336, .T. ) ;
#2316 = DIRECTION ( 'NONE',  ( -8.163404592832030268E-17, 1.000000000000000000, -0.000000000000000000 ) ) ;
#2317 = EDGE_CURVE ( 'NONE', #9984, #5834, #5992, .T. ) ;
#2318 = AXIS2_PLACEMENT_3D ( 'NONE', #9709, #1132, #11503 ) ;
#2319 = EDGE_CURVE ( 'NONE', #11283, #4655, #4613, .T. ) ;
#2320 = CARTESIAN_POINT ( 'NONE',  ( -210.0000000000000000, 139.9999999999999716, -126.4213562373080180 ) ) ;
#2321 = DIRECTION ( 'NONE',  ( 0.000000000000000000, 1.000000000000000000, -0.000000000000000000 ) ) ;
#2322 = TOROIDAL_SURFACE ( 'NONE', #10803, 44.00000000000000711, 1.000000000000000000 ) ;
#2323 = CARTESIAN_POINT ( 'NONE',  ( -993.6119331254994904, 96.30709745136255151, -96.78565065507915222 ) ) ;
#2324 = DIRECTION ( 'NONE',  ( -8.163404592832030268E-17, 1.000000000000000000, -0.000000000000000000 ) ) ;
#2325 = CARTESIAN_POINT ( 'NONE',  ( -19.93162290699157779, 178.2126347188217608, -126.3409196197182780 ) ) ;
#2326 = ORIENTED_EDGE ( 'NONE', *, *, #11602, .T. ) ;
#2327 = CIRCLE ( 'NONE', #8836, 7.500000000000007105 ) ;
#2328 = ORIENTED_EDGE ( 'NONE', *, *, #238, .T. ) ;
#2329 = CARTESIAN_POINT ( 'NONE',  ( -824.1625816070830979, 83.67410183576217264, -154.1030193367455468 ) ) ;
#2330 = CARTESIAN_POINT ( 'NONE',  ( -1055.176328965296989, 98.13059730676610570, -99.57582448894517313 ) ) ;
#2331 = CARTESIAN_POINT ( 'NONE',  ( 4.255174644013695128E-15, 25.00000000000002132, -126.4213562373094959 ) ) ;
#2332 = CARTESIAN_POINT ( 'NONE',  ( -1010.922847972425529, 120.6260792194948550, -124.6807709998039542 ) ) ;
#2333 = CARTESIAN_POINT ( 'NONE',  ( -142.5000000000000000, -9.213203435596451385, -126.4213562373084301 ) ) ;
#2334 = CARTESIAN_POINT ( 'NONE',  ( 19.97697870131679920, 180.4645185616454910, -126.1401451060182382 ) ) ;
#2335 = DIRECTION ( 'NONE',  ( 0.9501779778103252028, 0.000000000000000000, 0.3117078928809489669 ) ) ;
#2336 = CONICAL_SURFACE ( 'NONE', #7663, 5.035999999999999588, 0.7853981633974410625 ) ;
#2337 = AXIS2_PLACEMENT_3D ( 'NONE', #8289, #2518, #5294 ) ;
#2338 = CARTESIAN_POINT ( 'NONE',  ( -1021.913416468816195, 116.8879375517085890, -113.1262384684096673 ) ) ;
#2339 = DIRECTION ( 'NONE',  ( -1.000000000000000000, 0.000000000000000000, 0.000000000000000000 ) ) ;
#2340 = CARTESIAN_POINT ( 'NONE',  ( -154.5043356068770493, 12.00000000000000000, -94.56666130601601594 ) ) ;
#2341 = CARTESIAN_POINT ( 'NONE',  ( 126.4213562373094959, 0.000000000000000000, 7.500000000000007105 ) ) ;
#2342 = CARTESIAN_POINT ( 'NONE',  ( -370.6747336736685838, 106.2267788995130786, -113.0893085367774376 ) ) ;
#2343 = APPLICATION_CONTEXT ( 'automotive_design' ) ;
#2344 = CARTESIAN_POINT ( 'NONE',  ( -819.0912165218314840, 80.28194760164100785, -94.83880827393758750 ) ) ;
#2345 = AXIS2_PLACEMENT_3D ( 'NONE', #1500, #10714, #5261 ) ;
#2346 = CARTESIAN_POINT ( 'NONE',  ( -823.8285638327245124, 78.67432280806536937, -159.6807709998044800 ) ) ;
#2347 = EDGE_LOOP ( 'NONE', ( #8247, #110 ) ) ;
#2348 = DIRECTION ( 'NONE',  ( 0.000000000000000000, 0.000000000000000000, 1.000000000000000000 ) ) ;
#2349 = CARTESIAN_POINT ( 'NONE',  ( -926.5138833012656505, 125.7648744980332225, -126.6442663926294330 ) ) ;
#2350 = AXIS2_PLACEMENT_3D ( 'NONE', #12130, #4765, #3955 ) ;
#2351 = FACE_OUTER_BOUND ( 'NONE', #3276, .T. ) ;
#2352 = CYLINDRICAL_SURFACE ( 'NONE', #3013, 57.99999999999999289 ) ;
#2353 = ORIENTED_EDGE ( 'NONE', *, *, #2018, .T. ) ;
#2354 = AXIS2_PLACEMENT_3D ( 'NONE', #8145, #6171, #3369 ) ;
#2355 = EDGE_LOOP ( 'NONE', ( #11164, #6242, #4884, #6676 ) ) ;
#2356 = DIRECTION ( 'NONE',  ( -1.000000000000000000, 0.000000000000000000, 0.000000000000000000 ) ) ;
#2357 = CARTESIAN_POINT ( 'NONE',  ( -382.0060323104738700, 67.53962357491931812, -138.5094348483520150 ) ) ;
#2358 = CARTESIAN_POINT ( 'NONE',  ( -1062.096538105497302, 73.81465972843197676, -154.2940595301284930 ) ) ;
#2359 = CYLINDRICAL_SURFACE ( 'NONE', #10041, 7.500000000000007994 ) ;
#2360 = DIRECTION ( 'NONE',  ( 1.000000000000000000, 0.000000000000000000, -0.000000000000000000 ) ) ;
#2361 = CARTESIAN_POINT ( 'NONE',  ( -822.2256338312696471, 73.93538682641413118, -94.71157759278341359 ) ) ;
#2362 = FILL_AREA_STYLE ('',( #2597 ) ) ;
#2363 =( GEOMETRIC_REPRESENTATION_CONTEXT ( 3 ) GLOBAL_UNCERTAINTY_ASSIGNED_CONTEXT ( ( #10663 ) ) GLOBAL_UNIT_ASSIGNED_CONTEXT ( ( #230, #3198, #4081 ) ) REPRESENTATION_CONTEXT ( 'NONE', 'WORKASPACE' ) );
#2364 = ORIENTED_EDGE ( 'NONE', *, *, #6921, .T. ) ;
#2365 = CARTESIAN_POINT ( 'NONE',  ( -1016.863910020547223, 59.13213530333427315, -141.4553492942757487 ) ) ;
#2366 = ORIENTED_EDGE ( 'NONE', *, *, #7290, .F. ) ;
#2367 = CARTESIAN_POINT ( 'NONE',  ( 20.94507493758783312, 178.7564165339132103, -124.4539389338348911 ) ) ;
#2368 = EDGE_CURVE ( 'NONE', #4474, #3651, #4632, .T. ) ;
#2369 = CARTESIAN_POINT ( 'NONE',  ( -817.2011019090423360, 28.13185037056188875, -118.7903414690680250 ) ) ;
#2370 = EDGE_CURVE ( 'NONE', #10860, #918, #6195, .T. ) ;
#2371 = CARTESIAN_POINT ( 'NONE',  ( -379.6770763389447438, 101.1299400358934690, -118.8159555003075809 ) ) ;
#2372 = EDGE_LOOP ( 'NONE', ( #7598, #10524, #2572, #9505, #11703 ) ) ;
#2373 = EDGE_LOOP ( 'NONE', ( #10806, #8204, #9866 ) ) ;
#2374 = EDGE_CURVE ( 'NONE', #9074, #6366, #4813, .T. ) ;
#2375 = DIRECTION ( 'NONE',  ( -8.163404592832030268E-17, 1.000000000000000000, -0.000000000000000000 ) ) ;
#2376 = CARTESIAN_POINT ( 'NONE',  ( -1061.673215548682720, 86.58918783539685649, -95.06748246948023962 ) ) ;
#2377 = CARTESIAN_POINT ( 'NONE',  ( -19.90245853136579868, 178.5200732004545898, -126.6601217908411314 ) ) ;
#2378 = VERTEX_POINT ( 'NONE', #1764 ) ;
#2379 = VERTEX_POINT ( 'NONE', #13 ) ;
#2380 = CARTESIAN_POINT ( 'NONE',  ( -818.8285638327237166, 78.67432280806536937, -89.68077099980398259 ) ) ;
#2381 = ADVANCED_FACE ( 'NONE', ( #3596 ), #8362, .F. ) ;
#2382 =( LENGTH_UNIT ( ) NAMED_UNIT ( * ) SI_UNIT ( .MILLI., .METRE. ) );
#2383 = DIRECTION ( 'NONE',  ( 0.000000000000000000, 0.000000000000000000, 1.000000000000000000 ) ) ;
#2384 = EDGE_LOOP ( 'NONE', ( #173, #10384, #8616, #4301 ) ) ;
#2385 = DIRECTION ( 'NONE',  ( 0.7071067811865479058, 0.000000000000000000, 0.7071067811865472397 ) ) ;
#2386 = CARTESIAN_POINT ( 'NONE',  ( -902.8257469293350823, 84.21185948885704420, -95.06748246948052383 ) ) ;
#2387 = DIRECTION ( 'NONE',  ( -0.000000000000000000, -1.000000000000000000, -0.000000000000000000 ) ) ;
#2388 = CARTESIAN_POINT ( 'NONE',  ( -1060.756016675584760, 112.8516620848307355, -126.6442663926292056 ) ) ;
#2389 = DIRECTION ( 'NONE',  ( 0.000000000000000000, -1.156482317317870246E-16, 1.000000000000000000 ) ) ;
#2390 = CARTESIAN_POINT ( 'NONE',  ( -27.53136272649514993, 180.2041921146316099, -134.6807709998038547 ) ) ;
#2391 = CARTESIAN_POINT ( 'NONE',  ( -828.5765974139357013, 80.27527354417595973, -104.7529721962248601 ) ) ;
#2392 = CARTESIAN_POINT ( 'NONE',  ( 5.717472393966525317E-16, -0.8794428697676625051, -9.000000000000000000 ) ) ;
#2393 = EDGE_CURVE ( 'NONE', #10150, #7370, #11724, .T. ) ;
#2394 = FILL_AREA_STYLE ('',( #5928 ) ) ;
#2395 = ORIENTED_EDGE ( 'NONE', *, *, #3479, .F. ) ;
#2396 = CARTESIAN_POINT ( 'NONE',  ( 0.000000000000000000, 0.000000000000000000, 0.000000000000000000 ) ) ;
#2397 = CARTESIAN_POINT ( 'NONE',  ( -852.8274699693115508, 120.9962006285026774, -118.7903414690677124 ) ) ;
#2398 = CARTESIAN_POINT ( 'NONE',  ( 0.000000000000000000, 0.000000000000000000, 0.000000000000000000 ) ) ;
#2399 = CARTESIAN_POINT ( 'NONE',  ( -8.500000000000000000, 167.0000000000000000, -124.6807709998038405 ) ) ;
#2400 = CARTESIAN_POINT ( 'NONE',  ( -374.4047048906529653, 72.86532638985215726, -96.54417189472898997 ) ) ;
#2401 = CIRCLE ( 'NONE', #11871, 7.500000000000007105 ) ;
#2402 = DIRECTION ( 'NONE',  ( -0.7071067811865473507, 0.000000000000000000, 0.7071067811865477948 ) ) ;
#2403 = ORIENTED_EDGE ( 'NONE', *, *, #2933, .T. ) ;
#2404 = CARTESIAN_POINT ( 'NONE',  ( 20.71987187177683509, 180.3155698455967979, -123.3062602373065175 ) ) ;
#2405 = CIRCLE ( 'NONE', #7742, 45.00000000000001421 ) ;
#2406 = CARTESIAN_POINT ( 'NONE',  ( -380.4123712287169496, 64.19693960509795261, -133.8127555985722381 ) ) ;
#2407 = CARTESIAN_POINT ( 'NONE',  ( -1027.019426772554198, 78.04595964998465263, -154.2940595301285782 ) ) ;
#2408 = CARTESIAN_POINT ( 'NONE',  ( -828.7881391349023943, 78.01879388416071492, -144.2812265043196760 ) ) ;
#2409 = CARTESIAN_POINT ( 'NONE',  ( -373.6838828167635711, 95.52325971351345402, -150.4055153106844216 ) ) ;
#2410 = LINE ( 'NONE', #1491, #7985 ) ;
#2411 = CARTESIAN_POINT ( 'NONE',  ( -822.6980360219018849, 73.80108637340964606, -94.71426656347418316 ) ) ;
#2412 = ORIENTED_EDGE ( 'NONE', *, *, #6530, .T. ) ;
#2413 = CARTESIAN_POINT ( 'NONE',  ( -1025.595947590964442, 58.17469240935094632, -141.4553492942760329 ) ) ;
#2414 = AXIS2_PLACEMENT_3D ( 'NONE', #2699, #8405, #12169 ) ;
#2415 = ORIENTED_EDGE ( 'NONE', *, *, #5296, .F. ) ;
#2416 = ORIENTED_EDGE ( 'NONE', *, *, #8925, .T. ) ;
#2417 = CARTESIAN_POINT ( 'NONE',  ( -21.06257444491743414, 180.3615573004741464, -126.4218899470852762 ) ) ;
#2418 = CARTESIAN_POINT ( 'NONE',  ( -19.97506881502268428, 181.0839254472395510, -123.4722291287969114 ) ) ;
#2419 = CIRCLE ( 'NONE', #10913, 7.500000000000007105 ) ;
#2420 = ORIENTED_EDGE ( 'NONE', *, *, #9087, .T. ) ;
#2421 = CARTESIAN_POINT ( 'NONE',  ( -379.4946887727529656, 101.4434214888139820, -119.9580570101217916 ) ) ;
#2422 = ORIENTED_EDGE ( 'NONE', *, *, #4862, .F. ) ;
#2423 = ORIENTED_EDGE ( 'NONE', *, *, #121, .F. ) ;
#2424 = EDGE_CURVE ( 'NONE', #4637, #11949, #8947, .T. ) ;
#2425 = DIRECTION ( 'NONE',  ( -1.000000000000000000, -0.000000000000000000, -0.000000000000000000 ) ) ;
#2426 = CARTESIAN_POINT ( 'NONE',  ( 0.000000000000000000, 0.000000000000000000, 0.000000000000000000 ) ) ;
#2427 = EDGE_CURVE ( 'NONE', #9404, #1455, #6387, .T. ) ;
#2428 = VECTOR ( 'NONE', #10558, 1000.000000000000000 ) ;
#2429 = LINE ( 'NONE', #6209, #11195 ) ;
#2430 = CARTESIAN_POINT ( 'NONE',  ( -1056.106496161727136, 78.18408418063160070, -94.48732055948630659 ) ) ;
#2431 = DIRECTION ( 'NONE',  ( -0.7071067811865479058, 0.000000000000000000, -0.7071067811865472397 ) ) ;
#2432 = PLANE ( 'NONE',  #1018 ) ;
#2433 = CARTESIAN_POINT ( 'NONE',  ( -374.7331952787391174, 88.13045056185990234, -95.50322499346698635 ) ) ;
#2434 = ORIENTED_EDGE ( 'NONE', *, *, #12039, .F. ) ;
#2435 = DIRECTION ( 'NONE',  ( 2.040851148208007875E-17, -1.000000000000000000, -0.000000000000000000 ) ) ;
#2436 = EDGE_LOOP ( 'NONE', ( #386, #34 ) ) ;
#2437 = CARTESIAN_POINT ( 'NONE',  ( 2.186774452080127126E-12, -6.000000000000005329, 83.57864376269050410 ) ) ;
#2438 = CIRCLE ( 'NONE', #2645, 7.500000000000007105 ) ;
#2439 =( NAMED_UNIT ( * ) SI_UNIT ( $, .STERADIAN. ) SOLID_ANGLE_UNIT ( ) );
#2440 = ORIENTED_EDGE ( 'NONE', *, *, #2696, .T. ) ;
#2441 = DIRECTION ( 'NONE',  ( 0.000000000000000000, -1.000000000000000000, -7.930164461608263644E-17 ) ) ;
#2442 = CARTESIAN_POINT ( 'NONE',  ( -1015.825132819593136, 80.44428838836749662, -95.06748246948035330 ) ) ;
#2443 = CARTESIAN_POINT ( 'NONE',  ( 7.500000000000000000, -10.39230484541326405, 0.000000000000000000 ) ) ;
#2444 = ADVANCED_FACE ( 'NONE', ( #9574 ), #8710, .F. ) ;
#2445 = CARTESIAN_POINT ( 'NONE',  ( -21.06773542571745139, 180.9985192952500199, -126.2048741678526937 ) ) ;
#2446 = AXIS2_PLACEMENT_3D ( 'NONE', #9750, #11794, #6910 ) ;
#2447 = EDGE_CURVE ( 'NONE', #10609, #8307, #5789, .T. ) ;
#2448 = AXIS2_PLACEMENT_3D ( 'NONE', #7157, #1531, #728 ) ;
#2449 = AXIS2_PLACEMENT_3D ( 'NONE', #4231, #4414, #1334 ) ;
#2450 = CARTESIAN_POINT ( 'NONE',  ( -1014.007272717921069, 117.9006809476441049, -113.1262384684097526 ) ) ;
#2451 = CARTESIAN_POINT ( 'NONE',  ( -35.00000000000000000, -4.436643353671145300E-15, 81.78351099501843180 ) ) ;
#2452 = CARTESIAN_POINT ( 'NONE',  ( -19.96162039375556674, 182.2324071300824642, -123.4314723458560081 ) ) ;
#2453 = PLANE ( 'NONE',  #1333 ) ;
#2454 = CARTESIAN_POINT ( 'NONE',  ( -957.2086549536782059, 47.65337959301152893, -124.6807709998040679 ) ) ;
#2455 = VERTEX_POINT ( 'NONE', #7714 ) ;
#2456 = LINE ( 'NONE', #2638, #5868 ) ;
#2457 = CARTESIAN_POINT ( 'NONE',  ( -1030.931480980267906, 117.9615145441170654, -124.6807709998043521 ) ) ;
#2458 = AXIS2_PLACEMENT_3D ( 'NONE', #1153, #5835, #9787 ) ;
#2459 = CIRCLE ( 'NONE', #5417, 7.500000000000007105 ) ;
#2460 = LINE ( 'NONE', #8095, #4186 ) ;
#2461 = CARTESIAN_POINT ( 'NONE',  ( 6.899999999999999467, 1.502314598737159228E-15, -8.999999999999998224 ) ) ;
#2462 = DIRECTION ( 'NONE',  ( 0.000000000000000000, 1.000000000000000000, 0.000000000000000000 ) ) ;
#2463 = EDGE_CURVE ( 'NONE', #915, #1185, #9148, .T. ) ;
#2464 = ORIENTED_EDGE ( 'NONE', *, *, #10327, .T. ) ;
#2465 = EDGE_CURVE ( 'NONE', #5569, #6750, #1257, .T. ) ;
#2466 = ORIENTED_EDGE ( 'NONE', *, *, #4354, .F. ) ;
#2467 = CARTESIAN_POINT ( 'NONE',  ( 19.96002121859434553, 179.9932536262492135, -123.2030480363463028 ) ) ;
#2468 = CIRCLE ( 'NONE', #4264, 7.500000000000013323 ) ;
#2469 = CARTESIAN_POINT ( 'NONE',  ( 1.387778780781445676E-14, -494.9999999999998863, 133.9213562373095101 ) ) ;
#2470 = PLANE ( 'NONE',  #11143 ) ;
#2471 = CARTESIAN_POINT ( 'NONE',  ( -828.8285638327243987, 78.67432280806596623, -144.4023295390031194 ) ) ;
#2472 = CARTESIAN_POINT ( 'NONE',  ( 0.000000000000000000, 7.794228634059941818, -4.500000000000007994 ) ) ;
#2473 = CARTESIAN_POINT ( 'NONE',  ( -232.4999999999999716, 151.9999999999999716, -126.4213562373078190 ) ) ;
#2474 = DIRECTION ( 'NONE',  ( 0.000000000000000000, 1.632680918566399772E-14, -1.000000000000000000 ) ) ;
#2475 = FACE_OUTER_BOUND ( 'NONE', #11339, .T. ) ;
#2476 = CARTESIAN_POINT ( 'NONE',  ( -89.99999999999998579, -9.213203435596451385, -126.4213562373088564 ) ) ;
#2477 = VERTEX_POINT ( 'NONE', #992 ) ;
#2478 = CARTESIAN_POINT ( 'NONE',  ( -902.4158961391586899, 71.79205886009079052, -149.7857175106635736 ) ) ;
#2479 = CIRCLE ( 'NONE', #9785, 6.500000000000005329 ) ;
#2480 = ORIENTED_EDGE ( 'NONE', *, *, #5946, .F. ) ;
#2481 = ORIENTED_EDGE ( 'NONE', *, *, #3995, .F. ) ;
#2482 = CARTESIAN_POINT ( 'NONE',  ( 19.99771933579459926, 178.7804467691931052, -124.1722115321708628 ) ) ;
#2483 = CARTESIAN_POINT ( 'NONE',  ( -21.06305143384230760, 180.4613526592487176, -126.4076700800818287 ) ) ;
#2484 = EDGE_LOOP ( 'NONE', ( #12232, #10611, #7447, #9409 ) ) ;
#2485 = CARTESIAN_POINT ( 'NONE',  ( -370.2343257278625970, 56.60651921569737510, -116.8345502163405030 ) ) ;
#2486 = CARTESIAN_POINT ( 'NONE',  ( -379.7826593342579713, 100.9462791126746595, -118.2474210935536973 ) ) ;
#2487 = EDGE_LOOP ( 'NONE', ( #10512, #7994, #9213, #5958, #2585, #6915 ) ) ;
#2488 = CIRCLE ( 'NONE', #6244, 7.500000000000013323 ) ;
#2489 = EDGE_LOOP ( 'NONE', ( #2863, #8978, #5125, #1092 ) ) ;
#2490 = CARTESIAN_POINT ( 'NONE',  ( -976.2517683711890868, 35.25052392388818134, -126.6442663926290777 ) ) ;
#2491 = DIRECTION ( 'NONE',  ( 0.000000000000000000, 0.000000000000000000, 1.000000000000000000 ) ) ;
#2492 = AXIS2_PLACEMENT_3D ( 'NONE', #3606, #9245, #26 ) ;
#2493 = CARTESIAN_POINT ( 'NONE',  ( -1061.884876827091830, 80.20192378191423188, -94.48732055948617869 ) ) ;
#2494 = CARTESIAN_POINT ( 'NONE',  ( 8.099999999999999645, 0.000000000000000000, 0.000000000000000000 ) ) ;
#2495 = DIRECTION ( 'NONE',  ( -1.000000000000000000, 0.000000000000000000, 0.000000000000000000 ) ) ;
#2496 = EDGE_CURVE ( 'NONE', #8307, #10609, #9740, .T. ) ;
#2497 = CARTESIAN_POINT ( 'NONE',  ( -375.0052866622255010, 81.99894079391765445, -104.6528133239954457 ) ) ;
#2498 = ORIENTED_EDGE ( 'NONE', *, *, #2855, .F. ) ;
#2499 = DIRECTION ( 'NONE',  ( 1.000000000000000000, 0.000000000000000000, 0.000000000000000000 ) ) ;
#2500 = CARTESIAN_POINT ( 'NONE',  ( -18.99999999999999645, 168.0000000000000000, -124.6807709998038405 ) ) ;
#2501 = EDGE_LOOP ( 'NONE', ( #947, #7426, #10048, #10580, #9332 ) ) ;
#2502 = CARTESIAN_POINT ( 'NONE',  ( -822.6948441016551214, 83.54682639321367787, -154.1324994421172505 ) ) ;
#2503 = CARTESIAN_POINT ( 'NONE',  ( -1031.956718292106189, 74.21439239895558160, -95.06748246948035330 ) ) ;
#2504 = CIRCLE ( 'NONE', #2917, 7.500000000000007105 ) ;
#2505 = CARTESIAN_POINT ( 'NONE',  ( -126.4213562373094959, -6.000000000000000000, 2.255140518769849223E-14 ) ) ;
#2506 = CARTESIAN_POINT ( 'NONE',  ( -126.4213562373094959, 12.00000000000000000, 2.255140518769849223E-14 ) ) ;
#2507 = CARTESIAN_POINT ( 'NONE',  ( -21.06240745282773474, 180.3699811770686949, -126.4269926335236676 ) ) ;
#2508 = CARTESIAN_POINT ( 'NONE',  ( 87.04832655144112152, 0.000000000000000000, -225.4289243767383368 ) ) ;
#2509 = DIRECTION ( 'NONE',  ( 0.000000000000000000, 1.000000000000000000, 0.000000000000000000 ) ) ;
#2510 = CIRCLE ( 'NONE', #10419, 7.500000000000007105 ) ;
#2511 = FACE_BOUND ( 'NONE', #8042, .T. ) ;
#2512 = CARTESIAN_POINT ( 'NONE',  ( 2.186774452080127126E-12, -6.000000000000005329, 83.57864376269050410 ) ) ;
#2513 = EDGE_CURVE ( 'NONE', #9788, #7020, #11491, .T. ) ;
#2514 = VERTEX_POINT ( 'NONE', #4988 ) ;
#2515 = DIRECTION ( 'NONE',  ( 1.000000000000000000, 0.000000000000000000, 0.000000000000000000 ) ) ;
#2516 = CARTESIAN_POINT ( 'NONE',  ( -1060.756016675587944, 112.8516620848305934, -122.7172756069790864 ) ) ;
#2517 = CYLINDRICAL_SURFACE ( 'NONE', #10894, 7.500000000000007105 ) ;
#2518 = DIRECTION ( 'NONE',  ( -0.000000000000000000, -1.000000000000000000, -0.000000000000000000 ) ) ;
#2519 = PLANE ( 'NONE',  #5210 ) ;
#2520 = AXIS2_PLACEMENT_3D ( 'NONE', #11776, #7413, #805 ) ;
#2521 = CARTESIAN_POINT ( 'NONE',  ( 19.98597855131029988, 181.3192703522229863, -125.6808798714440343 ) ) ;
#2522 = ORIENTED_EDGE ( 'NONE', *, *, #8570, .T. ) ;
#2523 = CARTESIAN_POINT ( 'NONE',  ( -1045.864486809339724, 115.5688325305733741, -124.6807709998043663 ) ) ;
#2524 = AXIS2_PLACEMENT_3D ( 'NONE', #9806, #4310, #10509 ) ;
#2525 = CARTESIAN_POINT ( 'NONE',  ( -19.89130973751302989, 181.1405932345318206, -122.5976180991194155 ) ) ;
#2526 = CARTESIAN_POINT ( 'NONE',  ( -247.5000000000000000, -9.213203435596478030, -126.4213562373078190 ) ) ;
#2527 = CARTESIAN_POINT ( 'NONE',  ( -1024.256845364727496, 79.46673622094714062, -154.2940595301284930 ) ) ;
#2528 = CARTESIAN_POINT ( 'NONE',  ( -828.1715959468244819, 76.17590192436176721, -143.8160639703675940 ) ) ;
#2529 = CIRCLE ( 'NONE', #10245, 19.00000000000000000 ) ;
#2530 = DIRECTION ( 'NONE',  ( -2.081668171172161734E-17, -4.930380657631307143E-31, 1.000000000000000000 ) ) ;
#2531 = CARTESIAN_POINT ( 'NONE',  ( 0.000000000000000000, 7.794228634059941818, -4.500000000000007994 ) ) ;
#2532 = CARTESIAN_POINT ( 'NONE',  ( -952.6992609796615170, 94.45070821375009018, -154.2940595301278961 ) ) ;
#2533 = VERTEX_POINT ( 'NONE', #2101 ) ;
#2534 = CARTESIAN_POINT ( 'NONE',  ( -379.1619848709566440, 102.0000000000000142, -124.6807709998038405 ) ) ;
#2535 = EDGE_CURVE ( 'NONE', #2309, #4859, #1177, .T. ) ;
#2536 = VERTEX_POINT ( 'NONE', #2906 ) ;
#2537 = CARTESIAN_POINT ( 'NONE',  ( 3.123963502971610252E-13, 152.0000000000000000, -88.92135623730946747 ) ) ;
#2538 = CARTESIAN_POINT ( 'NONE',  ( -1032.260242496265846, 61.00429285198246987, -149.7857175106635452 ) ) ;
#2539 = VECTOR ( 'NONE', #5120, 1000.000000000000000 ) ;
#2540 = DIRECTION ( 'NONE',  ( -3.061276722312011504E-17, 1.000000000000000000, 0.000000000000000000 ) ) ;
#2541 = ORIENTED_EDGE ( 'NONE', *, *, #5149, .F. ) ;
#2542 = ADVANCED_FACE ( 'NONE', ( #4931 ), #226, .F. ) ;
#2543 = EDGE_CURVE ( 'NONE', #6290, #9223, #2054, .T. ) ;
#2544 = ORIENTED_EDGE ( 'NONE', *, *, #824, .T. ) ;
#2545 = CARTESIAN_POINT ( 'NONE',  ( -19.83130628892425307, 180.1366617011883307, -127.2729378191562120 ) ) ;
#2546 = ORIENTED_EDGE ( 'NONE', *, *, #11954, .F. ) ;
#2547 = CARTESIAN_POINT ( 'NONE',  ( -372.4042090581564253, 61.94512028621924316, -124.6876203640234451 ) ) ;
#2548 = VECTOR ( 'NONE', #6729, 1000.000000000000000 ) ;
#2549 = FACE_OUTER_BOUND ( 'NONE', #6948, .T. ) ;
#2550 = EDGE_LOOP ( 'NONE', ( #8471, #8703, #7056, #11086 ) ) ;
#2552 = EDGE_CURVE ( 'NONE', #822, #1329, #8388, .T. ) ;
#2551 = CARTESIAN_POINT ( 'NONE',  ( 2.498657532616778856E-14, -6.999999999999978684, -124.6807709998038405 ) ) ;
#2553 = ORIENTED_EDGE ( 'NONE', *, *, #11769, .F. ) ;
#2554 = CARTESIAN_POINT ( 'NONE',  ( 1.479627290717497352E-14, -494.9999999999998863, 118.9213562373094817 ) ) ;
#2555 = AXIS2_PLACEMENT_3D ( 'NONE', #8142, #7215, #10983 ) ;
#2556 = CARTESIAN_POINT ( 'NONE',  ( -151.3258811035894098, 12.00000000000000000, -56.13263083939680342 ) ) ;
#2557 = CARTESIAN_POINT ( 'NONE',  ( -823.8285638327247398, 78.67432280806536937, -158.6807709998041673 ) ) ;
#2558 = CARTESIAN_POINT ( 'NONE',  ( -974.9912860506733523, 88.33816101283738931, -95.06748246948018277 ) ) ;
#2559 = LINE ( 'NONE', #3476, #1426 ) ;
#2560 = ORIENTED_EDGE ( 'NONE', *, *, #6918, .F. ) ;
#2561 = FACE_OUTER_BOUND ( 'NONE', #4749, .T. ) ;
#2562 = CARTESIAN_POINT ( 'NONE',  ( 1.387778780781445676E-14, -494.9999999999998863, 126.4213562373094959 ) ) ;
#2563 = EDGE_LOOP ( 'NONE', ( #2112, #7915, #6425, #11031 ) ) ;
#2564 = CARTESIAN_POINT ( 'NONE',  ( -821.3240427761263618, 83.01413755802123262, -154.2176382493157121 ) ) ;
#2565 = CARTESIAN_POINT ( 'NONE',  ( -953.5758047008322364, 72.53746257253780527, -96.78565065507940801 ) ) ;
#2566 = CYLINDRICAL_SURFACE ( 'NONE', #4120, 7.500000000000012434 ) ;
#2567 = DIRECTION ( 'NONE',  ( -0.000000000000000000, 1.000000000000000000, 0.000000000000000000 ) ) ;
#2568 = CARTESIAN_POINT ( 'NONE',  ( -30.00000000000000000, 152.0000000000000000, -126.4213562373092685 ) ) ;
#2569 = CARTESIAN_POINT ( 'NONE',  ( 1.387778780781445676E-14, 152.0000000000000284, 126.4213562373094959 ) ) ;
#2570 = CARTESIAN_POINT ( 'NONE',  ( -20.71893962830172953, 180.2427088464574183, -123.3024896548053988 ) ) ;
#2571 = CARTESIAN_POINT ( 'NONE',  ( -828.8205192778966648, 78.34647195564905076, -144.3449412327537686 ) ) ;
#2572 = ORIENTED_EDGE ( 'NONE', *, *, #8792, .T. ) ;
#2573 = DIRECTION ( 'NONE',  ( 0.000000000000000000, 0.000000000000000000, -1.000000000000000000 ) ) ;
#2574 = CARTESIAN_POINT ( 'NONE',  ( -819.8516439069035187, 75.62621158465508131, -154.6795882100938400 ) ) ;
#2575 = ORIENTED_EDGE ( 'NONE', *, *, #6553, .T. ) ;
#2576 = FACE_OUTER_BOUND ( 'NONE', #4132, .T. ) ;
#2577 = CARTESIAN_POINT ( 'NONE',  ( -795.0000000000020464, 111.6133447792289530, -118.7903414690682524 ) ) ;
#2578 = CIRCLE ( 'NONE', #7719, 7.500000000000007105 ) ;
#2579 = DIRECTION ( 'NONE',  ( -0.000000000000000000, 1.000000000000000000, -0.000000000000000000 ) ) ;
#2580 = CARTESIAN_POINT ( 'NONE',  ( 2.510525938252074008E-14, -7.999999999999979572, -124.6807709998038405 ) ) ;
#2581 = EDGE_CURVE ( 'NONE', #6447, #5359, #2063, .T. ) ;
#2582 = CARTESIAN_POINT ( 'NONE',  ( 21.00015071161585212, 181.7073031029140679, -124.8819044078220060 ) ) ;
#2583 = EDGE_CURVE ( 'NONE', #11133, #2514, #6986, .T. ) ;
#2584 = ORIENTED_EDGE ( 'NONE', *, *, #616, .F. ) ;
#2585 = ORIENTED_EDGE ( 'NONE', *, *, #3685, .T. ) ;
#2586 = DIRECTION ( 'NONE',  ( -0.000000000000000000, 1.000000000000000000, -0.000000000000000000 ) ) ;
#2587 = LINE ( 'NONE', #12124, #11929 ) ;
#2588 = CARTESIAN_POINT ( 'NONE',  ( -1065.000000000004320, 98.77454568802519930, -149.7857175106631189 ) ) ;
#2589 = CARTESIAN_POINT ( 'NONE',  ( -379.2139264233433664, 101.9143973957450271, -126.6420371101448552 ) ) ;
#2590 = EDGE_CURVE ( 'NONE', #2717, #7665, #7502, .T. ) ;
#2591 = CYLINDRICAL_SURFACE ( 'NONE', #8082, 7.500000000000007105 ) ;
#2592 = DIRECTION ( 'NONE',  ( 0.000000000000000000, 0.000000000000000000, 1.000000000000000000 ) ) ;
#2593 = DIRECTION ( 'NONE',  ( -0.000000000000000000, 1.000000000000000000, 7.930164461608263644E-17 ) ) ;
#2594 = VERTEX_POINT ( 'NONE', #1295 ) ;
#2595 = CARTESIAN_POINT ( 'NONE',  ( -818.8285638327243987, 78.67432280806558254, -94.73795703228648790 ) ) ;
#2596 = AXIS2_PLACEMENT_3D ( 'NONE', #10863, #4270, #6178 ) ;
#2597 = FILL_AREA_STYLE_COLOUR ( '', #8264 ) ;
#2598 = EDGE_LOOP ( 'NONE', ( #12179, #695, #2648, #7263 ) ) ;
#2599 = LINE ( 'NONE', #5733, #729 ) ;
#2600 = CARTESIAN_POINT ( 'NONE',  ( -1024.256845364727496, 79.46673622094714062, -154.2940595301284930 ) ) ;
#2601 = CARTESIAN_POINT ( 'NONE',  ( 19.83591177254676907, 180.6622834474515003, -127.2381046240775646 ) ) ;
#2602 = VERTEX_POINT ( 'NONE', #1467 ) ;
#2603 = VERTEX_POINT ( 'NONE', #11854 ) ;
#2604 = AXIS2_PLACEMENT_3D ( 'NONE', #10062, #6293, #1656 ) ;
#2605 = EDGE_CURVE ( 'NONE', #10791, #818, #5424, .T. ) ;
#2606 = ORIENTED_EDGE ( 'NONE', *, *, #4478, .F. ) ;
#2607 = CARTESIAN_POINT ( 'NONE',  ( -371.2164454780093479, 59.29687532392634353, -139.7481348488436765 ) ) ;
#2608 = DIRECTION ( 'NONE',  ( 1.224646799147376133E-16, 1.000000000000000000, 4.955873740258437191E-31 ) ) ;
#2609 = EDGE_LOOP ( 'NONE', ( #3465, #10628, #4567, #1129 ) ) ;
#2610 = EDGE_CURVE ( 'NONE', #4244, #11206, #8395, .T. ) ;
#2611 = VERTEX_POINT ( 'NONE', #4631 ) ;
#2612 = DIRECTION ( 'NONE',  ( -0.000000000000000000, 1.000000000000000000, 7.930164461608263644E-17 ) ) ;
#2613 = FACE_OUTER_BOUND ( 'NONE', #2487, .T. ) ;
#2614 = DIRECTION ( 'NONE',  ( -3.061276722312011504E-17, 1.000000000000000000, 0.000000000000000000 ) ) ;
#2615 = EDGE_CURVE ( 'NONE', #6173, #4980, #11332, .T. ) ;
#2616 = CARTESIAN_POINT ( 'NONE',  ( -1015.517346982276649, 86.95624952299064603, -94.48732055948629238 ) ) ;
#2617 = CARTESIAN_POINT ( 'NONE',  ( -120.8820948793972434, 0.000000000000000000, -179.1989091883324363 ) ) ;
#2618 = DIRECTION ( 'NONE',  ( 2.081668171172161734E-17, 4.930380657631307143E-31, -1.000000000000000000 ) ) ;
#2619 = CARTESIAN_POINT ( 'NONE',  ( -825.4446906002115156, 83.41738352290740011, -144.6308861023095460 ) ) ;
#2620 = VERTEX_POINT ( 'NONE', #660 ) ;
#2621 = CARTESIAN_POINT ( 'NONE',  ( -822.2160636604378396, 83.41847921025862433, -144.6308011508168079 ) ) ;
#2622 = DIRECTION ( 'NONE',  ( 0.000000000000000000, 1.000000000000000000, 0.000000000000000000 ) ) ;
#2623 = ORIENTED_EDGE ( 'NONE', *, *, #2286, .T. ) ;
#2624 = CARTESIAN_POINT ( 'NONE',  ( 151.3258811035896656, 12.00000000000000000, -63.63263083939799003 ) ) ;
#2625 = CARTESIAN_POINT ( 'NONE',  ( -1032.113539130918525, 67.34854938887495734, -96.78565065507952170 ) ) ;
#2626 = AXIS2_PLACEMENT_3D ( 'NONE', #8056, #11078, #4287 ) ;
#2627 = CARTESIAN_POINT ( 'NONE',  ( -30.00000000000000000, -492.9999999999998863, 30.00000000000000000 ) ) ;
#2628 = DIRECTION ( 'NONE',  ( 0.000000000000000000, 0.000000000000000000, 1.000000000000000000 ) ) ;
#2629 = CARTESIAN_POINT ( 'NONE',  ( 126.4213562373094959, -6.000000000000000000, 7.500000000000006217 ) ) ;
#2630 = CARTESIAN_POINT ( 'NONE',  ( -824.9897882054046931, 73.80822682502996201, -106.4353286633422471 ) ) ;
#2631 = CARTESIAN_POINT ( 'NONE',  ( -19.99929956756464478, 178.7451710997399346, -124.2412955515236490 ) ) ;
#2632 = DIRECTION ( 'NONE',  ( -0.000000000000000000, 0.5000000000000009992, 0.8660254037844380415 ) ) ;
#2633 = AXIS2_PLACEMENT_3D ( 'NONE', #1340, #5039, #4175 ) ;
#2634 = ORIENTED_EDGE ( 'NONE', *, *, #1943, .F. ) ;
#2635 = ORIENTED_EDGE ( 'NONE', *, *, #10768, .T. ) ;
#2636 = PLANE ( 'NONE',  #6970 ) ;
#2637 = ORIENTED_EDGE ( 'NONE', *, *, #5912, .F. ) ;
#2638 = CARTESIAN_POINT ( 'NONE',  ( 45.53315400109643463, 12.00000000000000000, -230.3419396193597208 ) ) ;
#2639 = CARTESIAN_POINT ( 'NONE',  ( -1054.380968608931425, 114.0683136310379524, -124.6807709998043663 ) ) ;
#2640 = ADVANCED_BREP_SHAPE_REPRESENTATION ( '', ( #8029, #11957 ), #4670 ) ;
#2641 = CARTESIAN_POINT ( 'NONE',  ( 1.561981751485805177E-12, 152.0000000000000000, 31.07864376269052542 ) ) ;
#2642 = DIRECTION ( 'NONE',  ( -0.000000000000000000, -1.000000000000000000, -0.000000000000000000 ) ) ;
#2643 = CARTESIAN_POINT ( 'NONE',  ( -371.9152332062730579, 61.43342894527527420, -105.9795901510680096 ) ) ;
#2644 = VECTOR ( 'NONE', #6740, 1000.000000000000000 ) ;
#2645 = AXIS2_PLACEMENT_3D ( 'NONE', #2657, #9081, #4652 ) ;
#2646 = AXIS2_PLACEMENT_3D ( 'NONE', #3933, #4973, #9496 ) ;
#2647 = CARTESIAN_POINT ( 'NONE',  ( 19.89942126619322238, 181.8500073156368160, -126.6862962162580430 ) ) ;
#2648 = ORIENTED_EDGE ( 'NONE', *, *, #11838, .F. ) ;
#2649 = ORIENTED_EDGE ( 'NONE', *, *, #7463, .F. ) ;
#2650 = DIRECTION ( 'NONE',  ( -1.000000000000000000, 0.000000000000000000, 0.000000000000000000 ) ) ;
#2651 = CARTESIAN_POINT ( 'NONE',  ( -305.0000000000000568, 151.9999999999999716, -89.68077099980384048 ) ) ;
#2652 = CARTESIAN_POINT ( 'NONE',  ( -952.4132309232853686, 101.5728619241206161, -152.5758913445289409 ) ) ;
#2653 = CARTESIAN_POINT ( 'NONE',  ( -828.8205192779003028, 78.34647195564971867, -144.3449412327541665 ) ) ;
#2654 = EDGE_CURVE ( 'NONE', #4090, #11527, #10941, .T. ) ;
#2655 = CIRCLE ( 'NONE', #9167, 7.500000000000007105 ) ;
#2656 = CARTESIAN_POINT ( 'NONE',  ( 0.000000000000000000, 0.000000000000000000, 0.000000000000000000 ) ) ;
#2657 = CARTESIAN_POINT ( 'NONE',  ( -29.99999999999998579, 12.00000000000001776, -126.4213562373092685 ) ) ;
#2658 = AXIS2_PLACEMENT_3D ( 'NONE', #4296, #3402, #8912 ) ;
#2659 = CARTESIAN_POINT ( 'NONE',  ( -821.6815100408632588, 89.78153722040215712, -152.5758913445288840 ) ) ;
#2660 = CARTESIAN_POINT ( 'NONE',  ( 1.874378101782966050E-12, 0.000000000000000000, 53.57864376269050410 ) ) ;
#2661 = ORIENTED_EDGE ( 'NONE', *, *, #9929, .T. ) ;
#2662 = FACE_BOUND ( 'NONE', #3396, .T. ) ;
#2663 = ORIENTED_EDGE ( 'NONE', *, *, #9249, .F. ) ;
#2664 = CARTESIAN_POINT ( 'NONE',  ( -1055.176328965298808, 98.13059730676609149, -149.7857175106632326 ) ) ;
#2665 = CARTESIAN_POINT ( 'NONE',  ( -975.3893330992545998, 71.12659035875127245, -154.2940595301280950 ) ) ;
#2666 = ORIENTED_EDGE ( 'NONE', *, *, #5247, .T. ) ;
#2667 = VECTOR ( 'NONE', #5683, 1000.000000000000000 ) ;
#2668 = VECTOR ( 'NONE', #4589, 1000.000000000000000 ) ;
#2669 = VERTEX_POINT ( 'NONE', #9123 ) ;
#2670 = CARTESIAN_POINT ( 'NONE',  ( -19.97875451785945700, 179.6374628416406836, -126.0536791248172648 ) ) ;
#2671 = CARTESIAN_POINT ( 'NONE',  ( -67.49999999999998579, -9.213203435596451385, -126.4213562373090696 ) ) ;
#2672 = ORIENTED_EDGE ( 'NONE', *, *, #4894, .T. ) ;
#2673 = CARTESIAN_POINT ( 'NONE',  ( -373.9743428662257543, 68.72570060467459996, -139.7265316089925022 ) ) ;
#2674 = CARTESIAN_POINT ( 'NONE',  ( -27.99999999999999645, -492.9999999999998863, -27.99999999999999645 ) ) ;
#2675 = EDGE_CURVE ( 'NONE', #2042, #4719, #5008, .T. ) ;
#2676 = DIRECTION ( 'NONE',  ( -0.7071067811865473507, 0.000000000000000000, 0.7071067811865477948 ) ) ;
#2677 = AXIS2_PLACEMENT_3D ( 'NONE', #2690, #5717, #12164 ) ;
#2678 = ORIENTED_EDGE ( 'NONE', *, *, #10006, .F. ) ;
#2679 = DIRECTION ( 'NONE',  ( 0.000000000000000000, 0.000000000000000000, 1.000000000000000000 ) ) ;
#2680 = EDGE_CURVE ( 'NONE', #10476, #2514, #9189, .T. ) ;
#2681 = CARTESIAN_POINT ( 'NONE',  ( 0.3570196857253388201, -6.047589086024968807, 7.525268439705679491 ) ) ;
#2682 = CARTESIAN_POINT ( 'NONE',  ( 19.92363529031039704, 178.2952318472436843, -126.4314419646907766 ) ) ;
#2683 = VECTOR ( 'NONE', #11928, 1000.000000000000000 ) ;
#2684 = CARTESIAN_POINT ( 'NONE',  ( -1038.283672687642365, 64.16172732404288581, -96.78565065507946485 ) ) ;
#2685 = CARTESIAN_POINT ( 'NONE',  ( 0.000000000000000000, 12.00000000000000000, -224.6807709998039968 ) ) ;
#2686 = CARTESIAN_POINT ( 'NONE',  ( -825.1286147475053667, 83.51336106040547236, -144.6235354408674141 ) ) ;
#2687 = ORIENTED_EDGE ( 'NONE', *, *, #9320, .T. ) ;
#2688 = CARTESIAN_POINT ( 'NONE',  ( -826.8836092318784949, 82.64591421739807231, -144.6711677827315157 ) ) ;
#2689 =( NAMED_UNIT ( * ) SI_UNIT ( $, .STERADIAN. ) SOLID_ANGLE_UNIT ( ) );
#2690 = CARTESIAN_POINT ( 'NONE',  ( 7.653191805780027529E-16, 138.9999999999999716, -126.4213562373094959 ) ) ;
#2691 = DIRECTION ( 'NONE',  ( 0.000000000000000000, 1.000000000000000000, 0.000000000000000000 ) ) ;
#2692 = ORIENTED_EDGE ( 'NONE', *, *, #9999, .T. ) ;
#2693 = EDGE_CURVE ( 'NONE', #2214, #759, #4500, .T. ) ;
#2694 = DIRECTION ( 'NONE',  ( 0.000000000000000000, 1.000000000000000000, 0.000000000000000000 ) ) ;
#2695 = CARTESIAN_POINT ( 'NONE',  ( -1065.000000000002501, 60.65002596136933732, -103.3307627799636350 ) ) ;
#2696 = EDGE_CURVE ( 'NONE', #6669, #1396, #3834, .T. ) ;
#2697 = DIRECTION ( 'NONE',  ( 4.236366511936864528E-16, -1.000000000000000000, -5.522905491341393153E-16 ) ) ;
#2698 = LINE ( 'NONE', #12100, #10329 ) ;
#2699 = CARTESIAN_POINT ( 'NONE',  ( -795.0000000000043201, 82.00000000000039790, -124.6807709998041105 ) ) ;
#2700 = ADVANCED_FACE ( 'NONE', ( #10303 ), #10147, .T. ) ;
#2701 = FACE_OUTER_BOUND ( 'NONE', #2563, .T. ) ;
#2702 = CARTESIAN_POINT ( 'NONE',  ( -20.77690287681668480, 179.3967289902496134, -123.5488579070389790 ) ) ;
#2703 = CARTESIAN_POINT ( 'NONE',  ( -827.6116022231220768, 75.38889084172069488, -143.5581011396505744 ) ) ;
#2704 = ORIENTED_EDGE ( 'NONE', *, *, #2693, .F. ) ;
#2705 = EDGE_LOOP ( 'NONE', ( #11668, #3001, #2118, #8690 ) ) ;
#2706 = DIRECTION ( 'NONE',  ( -0.000000000000000000, 1.000000000000000000, 7.930164461608263644E-17 ) ) ;
#2707 = CARTESIAN_POINT ( 'NONE',  ( -373.6129858352072119, 95.87061353962586452, -99.20626003773914192 ) ) ;
#2708 = ORIENTED_EDGE ( 'NONE', *, *, #5618, .T. ) ;
#2709 = CARTESIAN_POINT ( 'NONE',  ( -974.3195816561840275, 116.7169707472884141, -107.9061927053320602 ) ) ;
#2710 = EDGE_CURVE ( 'NONE', #5191, #6316, #6595, .T. ) ;
#2711 = CARTESIAN_POINT ( 'NONE',  ( 126.4213562373094959, -6.000000000000000000, 7.500000000000006217 ) ) ;
#2712 = CARTESIAN_POINT ( 'NONE',  ( 2.186774452080127126E-12, -6.000000000000006217, 91.07864376269050410 ) ) ;
#2713 = CARTESIAN_POINT ( 'NONE',  ( 21.03739706409710308, 181.6552966610061333, -125.2847076232827277 ) ) ;
#2714 = VECTOR ( 'NONE', #1415, 1000.000000000000000 ) ;
#2715 = ORIENTED_EDGE ( 'NONE', *, *, #6765, .T. ) ;
#2716 = CIRCLE ( 'NONE', #6468, 7.500000000000007105 ) ;
#2717 = VERTEX_POINT ( 'NONE', #6411 ) ;
#2718 = CARTESIAN_POINT ( 'NONE',  ( -1010.922847972425529, 120.6260792194948550, -124.6807709998039542 ) ) ;
#2719 = DIRECTION ( 'NONE',  ( 0.3117078928809249860, 1.670400663243698742E-14, -0.9501779778103330854 ) ) ;
#2720 = FACE_OUTER_BOUND ( 'NONE', #9967, .T. ) ;
#2721 = CARTESIAN_POINT ( 'NONE',  ( -1025.595388641371756, 103.7168792382127975, -149.7857175106636021 ) ) ;
#2722 =( LENGTH_UNIT ( ) NAMED_UNIT ( * ) SI_UNIT ( .MILLI., .METRE. ) );
#2723 = CARTESIAN_POINT ( 'NONE',  ( 0.000000000000000000, 0.000000000000000000, -126.4213562373094959 ) ) ;
#2724 = CARTESIAN_POINT ( 'NONE',  ( -1031.632959140996718, 88.47632675500395294, -154.2940595301282087 ) ) ;
#2725 = FACE_OUTER_BOUND ( 'NONE', #1894, .T. ) ;
#2726 = EDGE_LOOP ( 'NONE', ( #3973, #10532 ) ) ;
#2727 = CARTESIAN_POINT ( 'NONE',  ( -828.8285638327245124, 78.67432280806571043, -264.6807709998050200 ) ) ;
#2728 = CARTESIAN_POINT ( 'NONE',  ( -247.5000000000000000, 12.00000000000001066, -126.4213562373078190 ) ) ;
#2729 = CARTESIAN_POINT ( 'NONE',  ( -373.8878671940757386, 94.45254164238392036, -151.1084388673575063 ) ) ;
#2730 = EDGE_LOOP ( 'NONE', ( #5594, #2095, #163, #11247 ) ) ;
#2731 = CARTESIAN_POINT ( 'NONE',  ( -1061.276350651670782, 98.40484402385492047, -149.7857175106635452 ) ) ;
#2732 = CARTESIAN_POINT ( 'NONE',  ( -955.9230626098308221, 78.80814421416198456, -154.2940595301282372 ) ) ;
#2733 = VERTEX_POINT ( 'NONE', #9062 ) ;
#2734 = AXIS2_PLACEMENT_3D ( 'NONE', #7147, #10795, #3307 ) ;
#2735 = ORIENTED_EDGE ( 'NONE', *, *, #11986, .F. ) ;
#2736 = AXIS2_PLACEMENT_3D ( 'NONE', #6664, #7654, #3697 ) ;
#2737 = CARTESIAN_POINT ( 'NONE',  ( -21.05155671971371945, 181.5816570678630058, -125.5021982045221023 ) ) ;
#2738 = CARTESIAN_POINT ( 'NONE',  ( -35.00000000000000000, 81.99999999999998579, 190.3192290001959748 ) ) ;
#2739 = CARTESIAN_POINT ( 'NONE',  ( -1065.000000000000909, 56.89504896194504369, -141.4553492942757771 ) ) ;
#2740 = ORIENTED_EDGE ( 'NONE', *, *, #68, .T. ) ;
#2741 = CARTESIAN_POINT ( 'NONE',  ( -371.0707588476642513, 58.87632496566943985, -138.8882774118476107 ) ) ;
#2742 = CARTESIAN_POINT ( 'NONE',  ( 126.4213562373094959, 12.00000000000000000, -6.938893903907228378E-15 ) ) ;
#2743 = FACE_OUTER_BOUND ( 'NONE', #9647, .T. ) ;
#2744 = ORIENTED_EDGE ( 'NONE', *, *, #10471, .T. ) ;
#2745 = VECTOR ( 'NONE', #11263, 1000.000000000000000 ) ;
#2746 = DIRECTION ( 'NONE',  ( -0.000000000000000000, 1.000000000000000000, 0.000000000000000000 ) ) ;
#2747 = EDGE_CURVE ( 'NONE', #4517, #11672, #275, .T. ) ;
#2748 = CARTESIAN_POINT ( 'NONE',  ( 0.000000000000000000, 0.000000000000000000, 9.000000000000000000 ) ) ;
#2749 = CARTESIAN_POINT ( 'NONE',  ( 19.95397453693550816, 178.0155092113254227, -126.0442809803723492 ) ) ;
#2750 = EDGE_CURVE ( 'NONE', #11221, #6923, #924, .T. ) ;
#2751 = CIRCLE ( 'NONE', #5707, 7.500000000000020428 ) ;
#2752 = CARTESIAN_POINT ( 'NONE',  ( -956.4793285278434496, 64.87563161486531271, -99.57582448894522997 ) ) ;
#2753 = CLOSED_SHELL ( 'NONE', ( #1911, #692, #446, #10635, #6145, #7798, #3072, #2700, #10898, #5576, #7681, #4206, #5538, #2249, #10033, #6300, #1852, #5079, #9343, #7282, #4928, #490, #11046, #3350, #6102, #2381, #1541, #7726, #5839, #2185, #6751 ) ) ;
#2754 = DIRECTION ( 'NONE',  ( 0.000000000000000000, 1.000000000000000000, 0.000000000000000000 ) ) ;
#2755 = LINE ( 'NONE', #5335, #9899 ) ;
#2756 = CARTESIAN_POINT ( 'NONE',  ( -379.2183536796136991, 101.9077751251720372, -126.8862509569658670 ) ) ;
#2757 = CARTESIAN_POINT ( 'NONE',  ( -991.8293279264742068, 119.7328159579556086, -136.2353035311976726 ) ) ;
#2758 = EDGE_LOOP ( 'NONE', ( #6588, #8120, #3553, #10029 ) ) ;
#2759 = CARTESIAN_POINT ( 'NONE',  ( -825.4446906002082187, 83.41738352290668956, -144.6308861023091197 ) ) ;
#2760 = EDGE_CURVE ( 'NONE', #8440, #6717, #10736, .T. ) ;
#2761 = CARTESIAN_POINT ( 'NONE',  ( -7.500000000000011546, 267.2792206135785591, -126.4213562373094959 ) ) ;
#2762 = EDGE_LOOP ( 'NONE', ( #10234, #2252 ) ) ;
#2763 = CARTESIAN_POINT ( 'NONE',  ( -1065.000000000009095, 65.22545431197600863, -99.57582448894517313 ) ) ;
#2764 = PLANE ( 'NONE',  #6482 ) ;
#2765 = VECTOR ( 'NONE', #6050, 1000.000000000000000 ) ;
#2766 = AXIS2_PLACEMENT_3D ( 'NONE', #2569, #11972, #722 ) ;
#2767 = CARTESIAN_POINT ( 'NONE',  ( -126.4213562373094959, -6.000000000000000000, -7.499999999999990230 ) ) ;
#2768 = FACE_OUTER_BOUND ( 'NONE', #666, .T. ) ;
#2769 = CARTESIAN_POINT ( 'NONE',  ( -825.6238610960850792, 74.00482032089485074, -106.3482309385107243 ) ) ;
#2770 = CARTESIAN_POINT ( 'NONE',  ( -19.88472492139865722, 179.4532041746028881, -122.5361950424904620 ) ) ;
#2771 = DIRECTION ( 'NONE',  ( -1.186840563529527301E-16, 1.000000000000000000, -0.000000000000000000 ) ) ;
#2772 = EDGE_CURVE ( 'NONE', #1708, #4712, #6773, .T. ) ;
#2773 = EDGE_LOOP ( 'NONE', ( #1327, #5628, #9622, #9159 ) ) ;
#2774 = CARTESIAN_POINT ( 'NONE',  ( -373.9906543607759772, 70.14504041414527080, -151.4544406809787347 ) ) ;
#2775 = CARTESIAN_POINT ( 'NONE',  ( -383.4148409544956166, 92.56808650636575919, -107.6977636917801533 ) ) ;
#2776 = EDGE_LOOP ( 'NONE', ( #9375, #9900, #37, #10500 ) ) ;
#2777 = CARTESIAN_POINT ( 'NONE',  ( -1031.197907781702725, 107.2697845108577894, -103.3307627799635640 ) ) ;
#2778 = DIRECTION ( 'NONE',  ( -2.081668171172161734E-17, -4.930380657631308019E-31, 1.000000000000000000 ) ) ;
#2779 = CARTESIAN_POINT ( 'NONE',  ( 19.98997306493104986, 181.4837338438134395, -125.4713928613115144 ) ) ;
#2780 = VERTEX_POINT ( 'NONE', #11292 ) ;
#2781 = ORIENTED_EDGE ( 'NONE', *, *, #7595, .T. ) ;
#2782 = ADVANCED_FACE ( 'NONE', ( #7583 ), #10426, .T. ) ;
#2783 = CARTESIAN_POINT ( 'NONE',  ( 13.32222501832767847, 180.2041921146325762, -184.1652315311843893 ) ) ;
#2784 = DIRECTION ( 'NONE',  ( 0.000000000000000000, 0.000000000000000000, 1.000000000000000000 ) ) ;
#2785 = CARTESIAN_POINT ( 'NONE',  ( -1015.209561144950953, 93.46821065761417913, -154.2940595301282656 ) ) ;
#2786 = DIRECTION ( 'NONE',  ( 0.000000000000000000, 0.000000000000000000, -1.000000000000000000 ) ) ;
#2787 = CARTESIAN_POINT ( 'NONE',  ( 9.184850993605159777E-16, -58.00000000000000711, -133.9213562373095101 ) ) ;
#2788 = SHAPE_REPRESENTATION_RELATIONSHIP ( 'NONE' , 'NONE' ,  #4488, #3228 ) ;
#2789 = EDGE_LOOP ( 'NONE', ( #5495, #7082 ) ) ;
#2790 = CARTESIAN_POINT ( 'NONE',  ( -827.8285638327238303, 78.67432280806536937, -89.68077099980398259 ) ) ;
#2791 = CARTESIAN_POINT ( 'NONE',  ( -383.0516306480785147, 93.70208505889323192, -140.9032205339583754 ) ) ;
#2792 = PRODUCT ( 'hex bolt gradeab_iso_ISO 4014 - M12 x 50 x 30-N', 'hex bolt gradeab_iso_ISO 4014 - M12 x 50 x 30-N', '', ( #5962 ) ) ;
#2793 = EDGE_LOOP ( 'NONE', ( #1256, #116 ) ) ;
#2794 = CARTESIAN_POINT ( 'NONE',  ( -1037.656130532295037, 99.96792753513321372, -149.7857175106633747 ) ) ;
#2795 = CARTESIAN_POINT ( 'NONE',  ( -1013.120138696094841, 73.26074010992857666, -152.5758913445291682 ) ) ;
#2796 = EDGE_LOOP ( 'NONE', ( #4764, #9890, #7885, #7728 ) ) ;
#2797 = ORIENTED_EDGE ( 'NONE', *, *, #5643, .F. ) ;
#2798 = CIRCLE ( 'NONE', #10491, 7.500000000000007105 ) ;
#2799 = CARTESIAN_POINT ( 'NONE',  ( -19.98689171310115853, 181.3620631069858007, -125.6334417695027525 ) ) ;
#2800 = FACE_BOUND ( 'NONE', #250, .T. ) ;
#2801 = CARTESIAN_POINT ( 'NONE',  ( -384.2952596656363085, 74.92966664680659505, -143.3922324125414320 ) ) ;
#2802 = DIRECTION ( 'NONE',  ( -0.7071067811865473507, -0.000000000000000000, 0.7071067811865477948 ) ) ;
#2803 = CARTESIAN_POINT ( 'NONE',  ( -384.5205618194315207, 76.13527207948695263, -105.5487487501123383 ) ) ;
#2804 = DIRECTION ( 'NONE',  ( -1.000000000000000000, 1.262554838833776231E-16, 0.000000000000000000 ) ) ;
#2805 = ORIENTED_EDGE ( 'NONE', *, *, #8944, .F. ) ;
#2806 = B_SPLINE_CURVE_WITH_KNOTS ( 'NONE', 3,
 ( #6647, #3604, #3866, #970, #8400, #2819, #7395, #784, #10415, #10238, #5597, #11167, #5534, #9308, #851, #1032, #9374, #10480, #1957, #6707, #4620, #4797, #917, #6587, #10355, #1897, #5660, #4741, #24, #5100, #9576, #2433, #8012, #9045, #514, #7136, #8655, #10901 ),
 .UNSPECIFIED., .F., .F.,
 ( 4, 2, 2, 2, 2, 2, 2, 2, 2, 2, 2, 2, 2, 2, 2, 2, 2, 2, 4 ),
 ( 0.1699018821680253755, 0.1767590822639642234, 0.1784733822879489284, 0.1801876823119336335, 0.1836162823599029603, 0.1870448824078722594, 0.1887591824318569367, 0.1904734824558415862, 0.1973306825517801288, 0.2007592825997494279, 0.2041878826477186992, 0.2076164826956879983, 0.2093307827196726478, 0.2110450827436572974, 0.2144736827916266242, 0.2179022828395959510, 0.2196165828635806005, 0.2213308828875652778, 0.2247594829355346324 ),
 .UNSPECIFIED. ) ;
#2807 = VECTOR ( 'NONE', #2462, 1000.000000000000000 ) ;
#2808 = DIRECTION ( 'NONE',  ( 0.000000000000000000, 0.000000000000000000, 1.000000000000000000 ) ) ;
#2809 = CARTESIAN_POINT ( 'NONE',  ( 21.06773055716234211, 179.3512387574996012, -126.1585967055013100 ) ) ;
#2810 = CIRCLE ( 'NONE', #9719, 7.500000000000007105 ) ;
#2811 = CARTESIAN_POINT ( 'NONE',  ( -1048.206790403141440, 45.99070412075073477, -107.9061927053325007 ) ) ;
#2812 = CARTESIAN_POINT ( 'NONE',  ( 45.53315400109643463, 12.00000000000000000, -245.3419396193597493 ) ) ;
#2813 = DIRECTION ( 'NONE',  ( 0.000000000000000000, 0.000000000000000000, 1.000000000000000000 ) ) ;
#2814 = CARTESIAN_POINT ( 'NONE',  ( -1057.805062346506702, 42.77845103615944566, -130.5712005305404944 ) ) ;
#2815 = TOROIDAL_SURFACE ( 'NONE', #9720, 19.00000000000000000, 1.000000000000000000 ) ;
#2816 = ORIENTED_EDGE ( 'NONE', *, *, #8640, .T. ) ;
#2817 = DIRECTION ( 'NONE',  ( 0.000000000000000000, 7.930164461608263644E-17, -1.000000000000000000 ) ) ;
#2818 = EDGE_CURVE ( 'NONE', #3744, #10023, #4640, .T. ) ;
#2819 = CARTESIAN_POINT ( 'NONE',  ( -369.8931053733606404, 108.2466269641216456, -125.4256155901781256 ) ) ;
#2820 = VERTEX_POINT ( 'NONE', #2828 ) ;
#2822 = ADVANCED_FACE ( 'NONE', ( #1902 ), #9442, .F. ) ;
#2821 = CARTESIAN_POINT ( 'NONE',  ( -1021.293373424897709, 59.24127555818995461, -107.9061927053327281 ) ) ;
#2823 = DIRECTION ( 'NONE',  ( -8.163404592832030268E-17, 1.000000000000000000, -0.000000000000000000 ) ) ;
#2824 = CARTESIAN_POINT ( 'NONE',  ( 1.874378101782966050E-12, 152.0000000000000000, 53.57864376269051832 ) ) ;
#2825 = PRODUCT_DEFINITION_CONTEXT ( 'detailed design', #2343, 'design' ) ;
#2826 = CIRCLE ( 'NONE', #9729, 8.999999999999998224 ) ;
#2827 = FACE_OUTER_BOUND ( 'NONE', #7106, .T. ) ;
#2828 = CARTESIAN_POINT ( 'NONE',  ( -375.0000000000000568, 81.99999999999994316, -154.6807709998039115 ) ) ;
#2829 = VERTEX_POINT ( 'NONE', #2023 ) ;
#2830 = DIRECTION ( 'NONE',  ( -0.000000000000000000, 1.000000000000000000, -0.000000000000000000 ) ) ;
#2831 = CONTEXT_DEPENDENT_SHAPE_REPRESENTATION ( #857, #6537 ) ;
#2832 = CARTESIAN_POINT ( 'NONE',  ( -372.5030970542207456, 100.5759890823530469, -103.3955147509480810 ) ) ;
#2833 = VECTOR ( 'NONE', #9248, 1000.000000000000000 ) ;
#2834 = ORIENTED_EDGE ( 'NONE', *, *, #6462, .T. ) ;
#2835 = EDGE_CURVE ( 'NONE', #9028, #7759, #11544, .T. ) ;
#2837 = EDGE_CURVE ( 'NONE', #559, #9851, #5396, .T. ) ;
#2836 = CARTESIAN_POINT ( 'NONE',  ( -1021.913416468816195, 116.8879375517085890, -113.1262384684096673 ) ) ;
#2838 = CARTESIAN_POINT ( 'NONE',  ( -35.00000000000000000, 152.0000000000000000, 190.3192290001959748 ) ) ;
#2839 = CARTESIAN_POINT ( 'NONE',  ( -6.097041784444755962E-13, 0.000000000000000000, -237.1807709998039115 ) ) ;
#2840 = EDGE_CURVE ( 'NONE', #1396, #6669, #3045, .T. ) ;
#2841 = CARTESIAN_POINT ( 'NONE',  ( 21.05611512818808961, 181.5525226013977260, -125.5803486369882478 ) ) ;
#2842 = AXIS2_PLACEMENT_3D ( 'NONE', #3082, #2035, #2161 ) ;
#2843 = CARTESIAN_POINT ( 'NONE',  ( -991.5701548301636876, 122.8678427087060214, -124.6807709998040536 ) ) ;
#2844 = ORIENTED_EDGE ( 'NONE', *, *, #9479, .F. ) ;
#2845 = DIRECTION ( 'NONE',  ( 0.000000000000000000, 1.000000000000000000, 0.000000000000000000 ) ) ;
#2846 = DIRECTION ( 'NONE',  ( 0.000000000000000000, 0.000000000000000000, 1.000000000000000000 ) ) ;
#2847 = CARTESIAN_POINT ( 'NONE',  ( -1031.632959140996718, 88.47632675500395294, -154.2940595301282087 ) ) ;
#2848 = DIRECTION ( 'NONE',  ( -0.000000000000000000, -0.000000000000000000, -1.000000000000000000 ) ) ;
#2849 = CARTESIAN_POINT ( 'NONE',  ( 57.50000000000000000, 6.757601037695094579E-16, -5.035999999999999588 ) ) ;
#2850 = ORIENTED_EDGE ( 'NONE', *, *, #740, .F. ) ;
#2851 = AXIS2_PLACEMENT_3D ( 'NONE', #11415, #6716, #1043 ) ;
#2852 = CARTESIAN_POINT ( 'NONE',  ( -1030.931480980266770, 117.9615145441171933, -126.6442663926290777 ) ) ;
#2853 = CIRCLE ( 'NONE', #9748, 7.500000000000007105 ) ;
#2854 = CARTESIAN_POINT ( 'NONE',  ( -381.0073242568000182, 98.64321884196588996, -135.7905410542184654 ) ) ;
#2855 = EDGE_CURVE ( 'NONE', #5146, #9369, #11014, .T. ) ;
#2856 = ORIENTED_EDGE ( 'NONE', *, *, #1704, .F. ) ;
#2857 = EDGE_CURVE ( 'NONE', #4489, #2055, #7391, .T. ) ;
#2858 = CARTESIAN_POINT ( 'NONE',  ( -1061.884876827093876, 80.20192378191431715, -154.8742214401230797 ) ) ;
#2859 = EDGE_CURVE ( 'NONE', #2594, #6370, #9222, .T. ) ;
#2860 = FACE_OUTER_BOUND ( 'NONE', #11455, .T. ) ;
#2861 = EDGE_LOOP ( 'NONE', ( #3338, #8774 ) ) ;
#2862 = CARTESIAN_POINT ( 'NONE',  ( -35.00000000000000000, 12.00000000000000000, 81.78351099501843180 ) ) ;
#2863 = ORIENTED_EDGE ( 'NONE', *, *, #10666, .F. ) ;
#2864 = VECTOR ( 'NONE', #11991, 1000.000000000000000 ) ;
#2865 = AXIS2_PLACEMENT_3D ( 'NONE', #8919, #10847, #9921 ) ;
#2866 = DIRECTION ( 'NONE',  ( 0.000000000000000000, 1.000000000000000000, -0.000000000000000000 ) ) ;
#2867 = VECTOR ( 'NONE', #10231, 1000.000000000000000 ) ;
#2868 = CARTESIAN_POINT ( 'NONE',  ( -825.1499223856457093, 73.84923531294217014, -106.4169293550704793 ) ) ;
#2869 = EDGE_LOOP ( 'NONE', ( #7671, #3456 ) ) ;
#2870 = CARTESIAN_POINT ( 'NONE',  ( -384.9074499709351471, 84.64590227528201183, -144.5159070364964577 ) ) ;
#2871 = FACE_OUTER_BOUND ( 'NONE', #10755, .T. ) ;
#2872 = CARTESIAN_POINT ( 'NONE',  ( -374.9921165712652282, 80.64358310894998283, -104.7226567718598034 ) ) ;
#2873 = DIRECTION ( 'NONE',  ( -0.000000000000000000, 1.000000000000000000, 7.930164461608263644E-17 ) ) ;
#2874 = AXIS2_PLACEMENT_3D ( 'NONE', #5585, #2746, #907 ) ;
#2875 = CARTESIAN_POINT ( 'NONE',  ( 0.000000000000000000, 12.00000000000001954, -124.6807709998040110 ) ) ;
#2876 = CARTESIAN_POINT ( 'NONE',  ( -1013.392840968506675, 67.31954129910425877, -99.57582448894551419 ) ) ;
#2877 = CARTESIAN_POINT ( 'NONE',  ( -828.8208027857029947, 78.99693817035523580, -104.9068376039975590 ) ) ;
#2878 = DIRECTION ( 'NONE',  ( -0.000000000000000000, 1.000000000000000000, -0.000000000000000000 ) ) ;
#2879 = CARTESIAN_POINT ( 'NONE',  ( -1021.607260580477828, 54.24386729702167997, -130.5712005305404659 ) ) ;
#2880 = COLOUR_RGB ( '', 0.72549020, 0.75294118, 0.79215686) ;
#2881 = CARTESIAN_POINT ( 'NONE',  ( -383.6153819378109802, 72.10737431220874782, -107.2890747853481912 ) ) ;
#2882 = ORIENTED_EDGE ( 'NONE', *, *, #959, .F. ) ;
#2883 = CARTESIAN_POINT ( 'NONE',  ( -820.7807412222807670, 82.64141399635636276, -144.6707558958800917 ) ) ;
#2884 = APPLICATION_PROTOCOL_DEFINITION ( 'draft international standard', 'automotive_design', 1998, #11196 ) ;
#2885 = LINE ( 'NONE', #9490, #11176 ) ;
#2886 = DIRECTION ( 'NONE',  ( 0.000000000000000000, -1.000000000000000000, 0.000000000000000000 ) ) ;
#2887 = ORIENTED_EDGE ( 'NONE', *, *, #3520, .F. ) ;
#2888 = DIRECTION ( 'NONE',  ( -8.163404592832030268E-17, 1.000000000000000000, -0.000000000000000000 ) ) ;
#2889 = CARTESIAN_POINT ( 'NONE',  ( -902.0880155070191222, 62.23309906011806447, -107.9061927053322876 ) ) ;
#2890 = DIRECTION ( 'NONE',  ( -0.000000000000000000, -0.000000000000000000, -1.000000000000000000 ) ) ;
#2891 = DIRECTION ( 'NONE',  ( 0.000000000000000000, -2.379049338482476554E-15, 1.000000000000000000 ) ) ;
#2892 =( GEOMETRIC_REPRESENTATION_CONTEXT ( 3 ) GLOBAL_UNCERTAINTY_ASSIGNED_CONTEXT ( ( #9795 ) ) GLOBAL_UNIT_ASSIGNED_CONTEXT ( ( #4176, #6096, #3300 ) ) REPRESENTATION_CONTEXT ( 'NONE', 'WORKASPACE' ) );
#2893 = EDGE_CURVE ( 'NONE', #8366, #10273, #9747, .T. ) ;
#2894 = CARTESIAN_POINT ( 'NONE',  ( -45.00000000000000711, 267.2792206135785591, -126.4213562373094959 ) ) ;
#2895 = ORIENTED_EDGE ( 'NONE', *, *, #5993, .T. ) ;
#2896 = CARTESIAN_POINT ( 'NONE',  ( -372.9914527493190235, 98.66121915142865362, -101.4780570701677931 ) ) ;
#2897 = ORIENTED_EDGE ( 'NONE', *, *, #1761, .F. ) ;
#2898 = CARTESIAN_POINT ( 'NONE',  ( -1011.418100375198719, 110.6663390795547599, -103.3307627799635782 ) ) ;
#2899 = AXIS2_PLACEMENT_3D ( 'NONE', #9260, #4572, #9195 ) ;
#2900 = DIRECTION ( 'NONE',  ( -1.000000000000000000, -0.000000000000000000, 0.000000000000000000 ) ) ;
#2901 = CARTESIAN_POINT ( 'NONE',  ( -823.1749794181308744, 110.1592441374104112, -141.4553492942763171 ) ) ;
#2902 = DIRECTION ( 'NONE',  ( -0.000000000000000000, -0.000000000000000000, -1.000000000000000000 ) ) ;
#2903 = EDGE_CURVE ( 'NONE', #11221, #8948, #1659, .T. ) ;
#2904 = CARTESIAN_POINT ( 'NONE',  ( -1037.337636019038882, 116.9882293220588991, -124.6807709998043521 ) ) ;
#2905 = ORIENTED_EDGE ( 'NONE', *, *, #1418, .F. ) ;
#2906 = CARTESIAN_POINT ( 'NONE',  ( -19.99999999999999645, 168.0000000000000000, -124.6807709998038405 ) ) ;
#2907 = EDGE_CURVE ( 'NONE', #1863, #83, #7787, .T. ) ;
#2908 = AXIS2_PLACEMENT_3D ( 'NONE', #6518, #8191, #11278 ) ;
#2909 = DIRECTION ( 'NONE',  ( 0.000000000000000000, 1.000000000000000000, -0.000000000000000000 ) ) ;
#2910 = PLANE ( 'NONE',  #10244 ) ;
#2911 = CARTESIAN_POINT ( 'NONE',  ( -1014.382386707152364, 110.5980896718283759, -146.0307792196445291 ) ) ;
#2912 = PLANE ( 'NONE',  #3232 ) ;
#2913 = DIRECTION ( 'NONE',  ( 0.000000000000000000, 0.000000000000000000, 1.000000000000000000 ) ) ;
#2914 = ORIENTED_EDGE ( 'NONE', *, *, #11535, .F. ) ;
#2915 = CARTESIAN_POINT ( 'NONE',  ( -374.7961310093019165, 88.54001489493019506, -143.6624644214829516 ) ) ;
#2916 = CARTESIAN_POINT ( 'NONE',  ( -1013.901471336339000, 119.8325901201404804, -130.5712005305404944 ) ) ;
#2917 = AXIS2_PLACEMENT_3D ( 'NONE', #8192, #5455, #9171 ) ;
#2918 = FACE_BOUND ( 'NONE', #890, .T. ) ;
#2919 = EDGE_LOOP ( 'NONE', ( #12184, #7238, #7706, #2 ) ) ;
#2920 = DIRECTION ( 'NONE',  ( 1.000000000000000000, 0.000000000000000000, 0.000000000000000000 ) ) ;
#2921 = VERTEX_POINT ( 'NONE', #10334 ) ;
#2922 = CARTESIAN_POINT ( 'NONE',  ( 1.387778780781445676E-14, 163.9999999999999716, 133.9213562373095101 ) ) ;
#2923 = CARTESIAN_POINT ( 'NONE',  ( -822.5144771496200065, 73.83866123373456958, -106.4215885538521178 ) ) ;
#2924 = CARTESIAN_POINT ( 'NONE',  ( -1021.046747802647246, 63.38047825189622841, -146.0307792196452681 ) ) ;
#2925 = ORIENTED_EDGE ( 'NONE', *, *, #616, .T. ) ;
#2926 =( GEOMETRIC_REPRESENTATION_CONTEXT ( 3 ) GLOBAL_UNCERTAINTY_ASSIGNED_CONTEXT ( ( #1276 ) ) GLOBAL_UNIT_ASSIGNED_CONTEXT ( ( #10584, #2241, #5947 ) ) REPRESENTATION_CONTEXT ( 'NONE', 'WORKASPACE' ) );
#2927 = EDGE_CURVE ( 'NONE', #10331, #7471, #6002, .T. ) ;
#2928 = CARTESIAN_POINT ( 'NONE',  ( -374.9190187245793595, 85.47274673630769826, -154.4334750548730710 ) ) ;
#2929 = CARTESIAN_POINT ( 'NONE',  ( 1.874378101782966050E-12, -6.000000000000005329, 53.57864376269050410 ) ) ;
#2930 = CARTESIAN_POINT ( 'NONE',  ( -374.8064248916637666, 75.73032293803038328, -105.6470633775803520 ) ) ;
#2931 = CARTESIAN_POINT ( 'NONE',  ( 45.00000000000000711, 267.2792206135785591, -126.4213562373094959 ) ) ;
#2932 = ORIENTED_EDGE ( 'NONE', *, *, #3197, .F. ) ;
#2933 = EDGE_CURVE ( 'NONE', #3651, #2975, #12075, .T. ) ;
#2934 = ORIENTED_EDGE ( 'NONE', *, *, #6014, .F. ) ;
#2935 = FACE_OUTER_BOUND ( 'NONE', #1143, .T. ) ;
#2936 = CARTESIAN_POINT ( 'NONE',  ( -1016.652307257391612, 63.31440937415304404, -103.3307627799640045 ) ) ;
#2937 = CARTESIAN_POINT ( 'NONE',  ( -818.9856806503992175, 79.95950042232037447, -104.7825536331199743 ) ) ;
#2938 = EDGE_LOOP ( 'NONE', ( #10127, #2672 ) ) ;
#2939 = EDGE_CURVE ( 'NONE', #206, #8172, #3231, .T. ) ;
#2940 = VECTOR ( 'NONE', #9312, 1000.000000000000000 ) ;
#2941 = CARTESIAN_POINT ( 'NONE',  ( -240.0000000000000000, -9.213203435596478030, -126.4213562373078190 ) ) ;
#2942 = ORIENTED_EDGE ( 'NONE', *, *, #8998, .T. ) ;
#2943 = CIRCLE ( 'NONE', #3928, 7.500000000000007105 ) ;
#2944 =( NAMED_UNIT ( * ) SI_UNIT ( $, .STERADIAN. ) SOLID_ANGLE_UNIT ( ) );
#2945 = ORIENTED_EDGE ( 'NONE', *, *, #9759, .F. ) ;
#2946 = CARTESIAN_POINT ( 'NONE',  ( -956.4793285278434496, 64.87563161486531271, -99.57582448894522997 ) ) ;
#2947 = CARTESIAN_POINT ( 'NONE',  ( -823.8285638327243987, 78.67432280806571043, -264.6807709998050200 ) ) ;
#2948 = DIRECTION ( 'NONE',  ( -0.9501779778103313090, 0.000000000000000000, -0.3117078928809301486 ) ) ;
#2949 = CARTESIAN_POINT ( 'NONE',  ( 20.00000000000000000, 197.0000000000000000, -124.6807709998038405 ) ) ;
#2950 = CIRCLE ( 'NONE', #976, 7.500000000000007105 ) ;
#2951 = UNCERTAINTY_MEASURE_WITH_UNIT (LENGTH_MEASURE( 1.000000000000000082E-05 ), #969, 'distance_accuracy_value', 'NONE');
#2952 = FACE_OUTER_BOUND ( 'NONE', #7516, .T. ) ;
#2953 = CARTESIAN_POINT ( 'NONE',  ( -19.98796572164149410, 179.0001281253265120, -125.5771477015080677 ) ) ;
#2954 = ORIENTED_EDGE ( 'NONE', *, *, #6853, .T. ) ;
#2955 = AXIS2_PLACEMENT_3D ( 'NONE', #1294, #7153, #5046 ) ;
#2956 = ORIENTED_EDGE ( 'NONE', *, *, #8524, .F. ) ;
#2957 = CARTESIAN_POINT ( 'NONE',  ( -1022.124201078493229, 113.7707856953083478, -107.9061927053324013 ) ) ;
#2958 = CARTESIAN_POINT ( 'NONE',  ( 0.5590800469813614892, -9.968355046870076563, -0.7343025909353910752 ) ) ;
#2959 = CARTESIAN_POINT ( 'NONE',  ( -45.53315400109751465, 12.00000000000000000, -230.3419396193594366 ) ) ;
#2960 = CARTESIAN_POINT ( 'NONE',  ( -795.0000000000047748, 112.0000000000007532, -124.6807709998042384 ) ) ;
#2961 = ORIENTED_EDGE ( 'NONE', *, *, #708, .F. ) ;
#2962 = DIRECTION ( 'NONE',  ( 1.000000000000000000, -1.262554838833776231E-16, 0.000000000000000000 ) ) ;
#2963 = DIRECTION ( 'NONE',  ( -8.163404592832030268E-17, 1.000000000000000000, -0.000000000000000000 ) ) ;
#2964 = DIRECTION ( 'NONE',  ( 0.000000000000000000, 0.000000000000000000, 1.000000000000000000 ) ) ;
#2965 = CARTESIAN_POINT ( 'NONE',  ( -1014.170783943998003, 114.7803637426474808, -141.4553492942763171 ) ) ;
#2966 = CARTESIAN_POINT ( 'NONE',  ( 141.4213562373095101, -494.9999999999998863, -1.508194112741312283E-14 ) ) ;
#2967 = CARTESIAN_POINT ( 'NONE',  ( -187.5000000000000000, -9.213203435596478030, -126.4213562373082453 ) ) ;
#2968 = FACE_OUTER_BOUND ( 'NONE', #3173, .T. ) ;
#2969 = ORIENTED_EDGE ( 'NONE', *, *, #1929, .F. ) ;
#2970 = EDGE_CURVE ( 'NONE', #9730, #178, #9103, .T. ) ;
#2971 = CARTESIAN_POINT ( 'NONE',  ( 19.97870119493365237, 182.4301677028706479, -123.7432126472026823 ) ) ;
#2972 = ADVANCED_FACE ( 'NONE', ( #5999, #5064, #128, #9769, #370, #1250, #7801, #5753, #308, #8608, #6805 ), #5874, .F. ) ;
#2973 = CARTESIAN_POINT ( 'NONE',  ( 1.387778780781445676E-14, -494.9999999999998863, 126.4213562373094959 ) ) ;
#2974 = ORIENTED_EDGE ( 'NONE', *, *, #4663, .T. ) ;
#2975 = VERTEX_POINT ( 'NONE', #4831 ) ;
#2976 = EDGE_CURVE ( 'NONE', #502, #5191, #1135, .T. ) ;
#2977 = DIRECTION ( 'NONE',  ( -0.000000000000000000, -0.000000000000000000, -1.000000000000000000 ) ) ;
#2978 = CARTESIAN_POINT ( 'NONE',  ( -21.06515428438344273, 181.3786429727620089, -125.8502496116465039 ) ) ;
#2979 = CARTESIAN_POINT ( 'NONE',  ( -819.0854767918264088, 77.05939038872190849, -105.2981374327915347 ) ) ;
#2980 = CARTESIAN_POINT ( 'NONE',  ( -954.2862664537763067, 55.36536439393486830, -141.4553492942758908 ) ) ;
#2981 = ORIENTED_EDGE ( 'NONE', *, *, #9759, .T. ) ;
#2982 = CARTESIAN_POINT ( 'NONE',  ( -374.9361197308762712, 78.97941656547077116, -154.4856030161737408 ) ) ;
#2983 = DIRECTION ( 'NONE',  ( -0.000000000000000000, 1.000000000000000000, 7.930164461608263644E-17 ) ) ;
#2984 = CARTESIAN_POINT ( 'NONE',  ( -374.9529056390816208, 78.74775624118257156, -104.9266946745538149 ) ) ;
#2985 = DIRECTION ( 'NONE',  ( 0.000000000000000000, 0.000000000000000000, 1.000000000000000000 ) ) ;
#2986 = CARTESIAN_POINT ( 'NONE',  ( 1.874378101782966050E-12, 163.9999999999999716, 53.57864376269051832 ) ) ;
#2987 = ORIENTED_EDGE ( 'NONE', *, *, #8338, .T. ) ;
#2988 = CARTESIAN_POINT ( 'NONE',  ( -817.2011019090375612, 28.13185037056175375, -130.5712005305403238 ) ) ;
#2989 = AXIS2_PLACEMENT_3D ( 'NONE', #3408, #10165, #645 ) ;
#2990 = ORIENTED_EDGE ( 'NONE', *, *, #47, .T. ) ;
#2991 = EDGE_CURVE ( 'NONE', #1810, #864, #4844, .T. ) ;
#2992 = CARTESIAN_POINT ( 'NONE',  ( -45.53315400109751465, 12.00000000000000000, -245.3419396193594650 ) ) ;
#2993 = CARTESIAN_POINT ( 'NONE',  ( -1013.120138696091999, 73.26074010992823560, -96.78565065507963538 ) ) ;
#2994 = CARTESIAN_POINT ( 'NONE',  ( -828.7652305532269565, 79.48420453549685760, -104.8389787515932881 ) ) ;
#2995 = LINE ( 'NONE', #3794, #4830 ) ;
#2996 = PRODUCT_RELATED_PRODUCT_CATEGORY ( 'part', '', ( #8619 ) ) ;
#2997 = VERTEX_POINT ( 'NONE', #8953 ) ;
#2998 = CARTESIAN_POINT ( 'NONE',  ( -382.1835803329706209, 67.94417042495855696, -110.4054994893419916 ) ) ;
#2999 = CARTESIAN_POINT ( 'NONE',  ( 1.561981751485805177E-12, 0.000000000000000000, 31.07864376269051121 ) ) ;
#3000 = LINE ( 'NONE', #8564, #8478 ) ;
#3001 = ORIENTED_EDGE ( 'NONE', *, *, #8640, .F. ) ;
#3002 = APPLICATION_PROTOCOL_DEFINITION ( 'draft international standard', 'automotive_design', 1998, #9295 ) ;
#3003 = ORIENTED_EDGE ( 'NONE', *, *, #9097, .F. ) ;
#3004 = AXIS2_PLACEMENT_3D ( 'NONE', #8878, #7964, #7026 ) ;
#3005 = CARTESIAN_POINT ( 'NONE',  ( -957.1839320239914741, 48.17551948191501765, -118.7903414690682951 ) ) ;
#3006 = DIRECTION ( 'NONE',  ( 1.000000000000000000, -1.026341648675396322E-47, 2.081668171172161734E-17 ) ) ;
#3007 = B_SPLINE_CURVE_WITH_KNOTS ( 'NONE', 3,
 ( #4963, #4452, #3505, #677, #10012, #7297, #11588, #2189, #1322, #4330, #3109, #9668, #9723, #6882, #7878, #1261, #8100, #8741, #1206, #5956 ),
 .UNSPECIFIED., .F., .F.,
 ( 4, 2, 2, 2, 2, 2, 2, 2, 2, 4 ),
 ( 0.0001175641502471066547, 0.0008018704293974582287, 0.001486176708547809911, 0.002170482987698161160, 0.002854789266848512842, 0.003539095545998864525, 0.004223401825149216207, 0.004907708104299568323, 0.005249861243874702314, 0.005592014383449837173 ),
 .UNSPECIFIED. ) ;
#3008 = DIRECTION ( 'NONE',  ( 0.3117078928809249860, 1.670400663243698742E-14, -0.9501779778103330854 ) ) ;
#3009 = ADVANCED_FACE ( 'NONE', ( #2290, #6124, #11756, #484, #3451, #6183, #9077, #9013, #613, #9949 ), #2470, .F. ) ;
#3010 = CIRCLE ( 'NONE', #6162, 1.000000000000000000 ) ;
#3011 = CARTESIAN_POINT ( 'NONE',  ( -904.0006525278403160, 119.6095687608906672, -107.9061927053323160 ) ) ;
#3012 = CARTESIAN_POINT ( 'NONE',  ( -818.8614508132078527, 78.01542073698732338, -105.0789755614316761 ) ) ;
#3013 = AXIS2_PLACEMENT_3D ( 'NONE', #7920, #11806, #10752 ) ;
#3014 = ORIENTED_EDGE ( 'NONE', *, *, #11620, .T. ) ;
#3015 = DIRECTION ( 'NONE',  ( 1.000000000000000000, 0.000000000000000000, 0.000000000000000000 ) ) ;
#3016 = CARTESIAN_POINT ( 'NONE',  ( -384.6663941904715784, 86.87630725089890404, -105.2815105480247411 ) ) ;
#3017 = ORIENTED_EDGE ( 'NONE', *, *, #3788, .T. ) ;
#3018 = CARTESIAN_POINT ( 'NONE',  ( -1046.457602311629898, 98.67849639484570901, -99.57582448894517313 ) ) ;
#3019 = CARTESIAN_POINT ( 'NONE',  ( -1017.840614713428863, 119.3387310954208118, -130.5712005305402954 ) ) ;
#3020 = AXIS2_PLACEMENT_3D ( 'NONE', #4543, #11151, #3464 ) ;
#3021 = CARTESIAN_POINT ( 'NONE',  ( -823.7697810748813936, 117.7733807739867871, -122.7172756069790438 ) ) ;
#3022 = VERTEX_POINT ( 'NONE', #5361 ) ;
#3023 = CARTESIAN_POINT ( 'NONE',  ( 7.653191805780027529E-16, 139.9999999999999716, -126.4213562373094959 ) ) ;
#3024 = DIRECTION ( 'NONE',  ( -0.000000000000000000, -1.000000000000000000, -0.000000000000000000 ) ) ;
#3025 = CARTESIAN_POINT ( 'NONE',  ( 154.5043356068769071, 12.00000000000000000, -102.0666613060171386 ) ) ;
#3026 = LINE ( 'NONE', #5624, #10749 ) ;
#3027 = CARTESIAN_POINT ( 'NONE',  ( -240.0000000000000000, 139.9999999999999716, -126.4213562373078190 ) ) ;
#3028 = CARTESIAN_POINT ( 'NONE',  ( -1065.000000000003411, 103.3499740386315580, -146.0307792196444154 ) ) ;
#3029 = CIRCLE ( 'NONE', #9931, 7.500000000000007105 ) ;
#3030 = CARTESIAN_POINT ( 'NONE',  ( 0.000000000000000000, 164.0000000000000000, -118.9213562373094817 ) ) ;
#3031 = ORIENTED_EDGE ( 'NONE', *, *, #8003, .F. ) ;
#3032 = ORIENTED_EDGE ( 'NONE', *, *, #6284, .F. ) ;
#3033 = EDGE_CURVE ( 'NONE', #2921, #4476, #10815, .T. ) ;
#3034 = CARTESIAN_POINT ( 'NONE',  ( 0.000000000000000000, 0.000000000000000000, -89.68077099980401101 ) ) ;
#3035 = CARTESIAN_POINT ( 'NONE',  ( -383.3143487999271883, 92.90250092716235031, -141.4580426032642890 ) ) ;
#3036 = CARTESIAN_POINT ( 'NONE',  ( 35.00000000000000000, 81.99999999999998579, 190.3192290001959748 ) ) ;
#3037 = CARTESIAN_POINT ( 'NONE',  ( -1062.301584968959560, 67.66927912025090563, -152.5758913445295377 ) ) ;
#3038 = ORIENTED_EDGE ( 'NONE', *, *, #11746, .T. ) ;
#3039 = CARTESIAN_POINT ( 'NONE',  ( -374.8641704781214230, 87.44069632558799299, -143.9908328712743071 ) ) ;
#3040 = CARTESIAN_POINT ( 'NONE',  ( -247.5000000000000000, 151.9999999999999716, -126.4213562373078190 ) ) ;
#3041 = CARTESIAN_POINT ( 'NONE',  ( -374.8592969718704353, 76.56519391583682932, -105.3927423586616499 ) ) ;
#3042 = CARTESIAN_POINT ( 'NONE',  ( 6.899999999999999467, -7.794228634059948924, -4.499999999999995559 ) ) ;
#3043 = ORIENTED_EDGE ( 'NONE', *, *, #9421, .F. ) ;
#3044 = CARTESIAN_POINT ( 'NONE',  ( -1021.483947769362658, 56.15424078096121008, -136.2353035311990368 ) ) ;
#3045 = CIRCLE ( 'NONE', #74, 7.500000000000007105 ) ;
#3046 = ORIENTED_EDGE ( 'NONE', *, *, #10330, .T. ) ;
#3047 = VECTOR ( 'NONE', #1183, 1000.000000000000000 ) ;
#3048 = CIRCLE ( 'NONE', #463, 7.500000000000007105 ) ;
#3049 = DIRECTION ( 'NONE',  ( -0.000000000000000000, 1.000000000000000000, -0.000000000000000000 ) ) ;
#3050 = CARTESIAN_POINT ( 'NONE',  ( 19.99672548776941383, 177.7005832697889787, -125.1535681142731420 ) ) ;
#3051 = CARTESIAN_POINT ( 'NONE',  ( -1062.923339974269538, 49.86928741160662071, -113.1262384684094968 ) ) ;
#3052 = CARTESIAN_POINT ( 'NONE',  ( -363.0000000000000568, 81.99999999999995737, -159.6807709998038547 ) ) ;
#3053 = EDGE_CURVE ( 'NONE', #7042, #5557, #8955, .T. ) ;
#3054 = VERTEX_POINT ( 'NONE', #3380 ) ;
#3055 = CARTESIAN_POINT ( 'NONE',  ( -384.9712557181327952, 80.53912230241294878, -104.7319216108211037 ) ) ;
#3056 = CARTESIAN_POINT ( 'NONE',  ( -826.4716404759357147, 74.42688921697002513, -154.6727229035019775 ) ) ;
#3057 = ORIENTED_EDGE ( 'NONE', *, *, #165, .T. ) ;
#3058 = CIRCLE ( 'NONE', #905, 7.500000000000007105 ) ;
#3059 = PRODUCT_CONTEXT ( 'NONE', #4004, 'mechanical' ) ;
#3060 = VECTOR ( 'NONE', #8488, 1000.000000000000000 ) ;
#3061 = ORIENTED_EDGE ( 'NONE', *, *, #10937, .F. ) ;
#3062 = CARTESIAN_POINT ( 'NONE',  ( -1032.658196452834773, 44.72920460984212809, -122.7172756069792143 ) ) ;
#3063 = CARTESIAN_POINT ( 'NONE',  ( -52.49999999999997868, -9.213203435596451385, -126.4213562373090696 ) ) ;
#3064 = CARTESIAN_POINT ( 'NONE',  ( -277.5000000000000000, 24.00000000000000711, -126.4213562373076059 ) ) ;
#3065 = FACE_BOUND ( 'NONE', #5038, .T. ) ;
#3066 = AXIS2_PLACEMENT_3D ( 'NONE', #11833, #5521, #2676 ) ;
#3067 = AXIS2_PLACEMENT_3D ( 'NONE', #2169, #8937, #6051 ) ;
#3068 = CARTESIAN_POINT ( 'NONE',  ( -1011.211222789223370, 114.9684118750912489, -107.9061927053323870 ) ) ;
#3069 = DIRECTION ( 'NONE',  ( 0.000000000000000000, 1.000000000000000000, 0.000000000000000000 ) ) ;
#3070 = ORIENTED_EDGE ( 'NONE', *, *, #11211, .F. ) ;
#3071 = DIRECTION ( 'NONE',  ( 0.000000000000000000, 0.000000000000000000, 1.000000000000000000 ) ) ;
#3072 = ADVANCED_FACE ( 'NONE', ( #11865 ), #12139, .T. ) ;
#3073 = ORIENTED_EDGE ( 'NONE', *, *, #10401, .T. ) ;
#3074 = CARTESIAN_POINT ( 'NONE',  ( -1022.719357623492556, 104.5170332807322922, -99.57582448894488891 ) ) ;
#3075 = VERTEX_POINT ( 'NONE', #11927 ) ;
#3076 = CARTESIAN_POINT ( 'NONE',  ( -262.5000000000000000, 12.00000000000001066, -126.4213562373076059 ) ) ;
#3077 = EDGE_CURVE ( 'NONE', #10083, #6258, #10939, .T. ) ;
#3078 = EDGE_CURVE ( 'NONE', #7692, #2455, #9370, .T. ) ;
#3079 = CARTESIAN_POINT ( 'NONE',  ( 19.91065551487656293, 178.8801318698700129, -122.7901100908945011 ) ) ;
#3080 = CARTESIAN_POINT ( 'NONE',  ( -19.98803719849065885, 181.4113409838737425, -123.7644832658072289 ) ) ;
#3081 = ORIENTED_EDGE ( 'NONE', *, *, #86, .T. ) ;
#3082 = CARTESIAN_POINT ( 'NONE',  ( 120.8820948793965186, 12.00000000000000000, -186.6989091883332890 ) ) ;
#3083 = CARTESIAN_POINT ( 'NONE',  ( -150.0000000000000000, 152.0000000000000000, -126.4213562373084301 ) ) ;
#3084 = CARTESIAN_POINT ( 'NONE',  ( -6.360897667028196044E-14, 0.000000000000000000, -141.4213562373094817 ) ) ;
#3085 = CARTESIAN_POINT ( 'NONE',  ( -1021.913416468810851, 116.8879375517085464, -136.2353035311978431 ) ) ;
#3086 = VECTOR ( 'NONE', #6084, 1000.000000000000000 ) ;
#3087 = EDGE_CURVE ( 'NONE', #8251, #2602, #5500, .T. ) ;
#3088 = CARTESIAN_POINT ( 'NONE',  ( -144.0488662551579182, 12.00000000000000000, -154.4077238332691877 ) ) ;
#3089 = CARTESIAN_POINT ( 'NONE',  ( -20.71964524312745937, 180.2041921146310415, -123.3053720114591272 ) ) ;
#3090 =( LENGTH_UNIT ( ) NAMED_UNIT ( * ) SI_UNIT ( .MILLI., .METRE. ) );
#3091 = ORIENTED_EDGE ( 'NONE', *, *, #10450, .T. ) ;
#3092 = CARTESIAN_POINT ( 'NONE',  ( 7.653191805780027529E-16, 139.9999999999999716, -82.42135623730948168 ) ) ;
#3093 = CARTESIAN_POINT ( 'NONE',  ( -1024.691966601152672, 118.8493250655916142, -124.6807709998039400 ) ) ;
#3094 = PRODUCT_DEFINITION_SHAPE ( 'NONE', 'NONE',  #12243 ) ;
#3095 = CARTESIAN_POINT ( 'NONE',  ( -795.0000000000046612, 103.3499740386315864, -146.0307792196441312 ) ) ;
#3096 = FACE_OUTER_BOUND ( 'NONE', #3647, .T. ) ;
#3097 = EDGE_LOOP ( 'NONE', ( #1879, #2740 ) ) ;
#3098 = AXIS2_PLACEMENT_3D ( 'NONE', #11073, #10143, #5436 ) ;
#3099 = ORIENTED_EDGE ( 'NONE', *, *, #2680, .T. ) ;
#3100 = CARTESIAN_POINT ( 'NONE',  ( -384.3668374026304946, 88.71950051914814139, -143.5273393398276198 ) ) ;
#3101 = CARTESIAN_POINT ( 'NONE',  ( -1032.391769651406321, 55.42093464310143247, -146.0307792196449839 ) ) ;
#3102 = CARTESIAN_POINT ( 'NONE',  ( 9.371890508914830252E-13, 12.00000000000000000, -36.42135623730949590 ) ) ;
#3103 = CARTESIAN_POINT ( 'NONE',  ( 2.186774452080127126E-12, 163.9999999999999716, 91.07864376269051832 ) ) ;
#3104 = TOROIDAL_SURFACE ( 'NONE', #136, 4.000000000000045297, 1.000000000000000000 ) ;
#3105 = ORIENTED_EDGE ( 'NONE', *, *, #1312, .T. ) ;
#3106 = ORIENTED_EDGE ( 'NONE', *, *, #8707, .T. ) ;
#3107 = DIRECTION ( 'NONE',  ( 0.000000000000000000, 5.522905491341382306E-16, 1.000000000000000000 ) ) ;
#3108 = CARTESIAN_POINT ( 'NONE',  ( -976.1667687410197232, 38.51511931707989334, -113.1262384684093263 ) ) ;
#3109 = CARTESIAN_POINT ( 'NONE',  ( -19.89960222275902524, 181.8553529586133379, -126.6887416412435243 ) ) ;
#3110 = CARTESIAN_POINT ( 'NONE',  ( -382.8339495845497709, 94.33502485403373328, -108.9270999018330173 ) ) ;
#3111 = EDGE_LOOP ( 'NONE', ( #1511, #11316, #1532, #10987 ) ) ;
#3112 = CARTESIAN_POINT ( 'NONE',  ( -823.5011105148523711, 73.67440276501611152, -154.6460142633133614 ) ) ;
#3113 = ORIENTED_EDGE ( 'NONE', *, *, #7922, .F. ) ;
#3114 = APPLICATION_PROTOCOL_DEFINITION ( 'draft international standard', 'automotive_design', 1998, #9041 ) ;
#3115 = ORIENTED_EDGE ( 'NONE', *, *, #8190, .T. ) ;
#3116 = CARTESIAN_POINT ( 'NONE',  ( -954.5692209181586350, 49.02792041507773746, -122.7172756069790580 ) ) ;
#3117 = AXIS2_PLACEMENT_3D ( 'NONE', #11424, #6484, #5490 ) ;
#3118 = EDGE_CURVE ( 'NONE', #4288, #7504, #6490, .T. ) ;
#3119 = CARTESIAN_POINT ( 'NONE',  ( -35.00000000000000000, 81.99999999999998579, 272.3192290001959464 ) ) ;
#3120 = CARTESIAN_POINT ( 'NONE',  ( 6.153765096826357259E-15, 138.9999999999999716, -170.4213562373095101 ) ) ;
#3121 = EDGE_CURVE ( 'NONE', #5146, #9670, #5013, .T. ) ;
#3122 = AXIS2_PLACEMENT_3D ( 'NONE', #9247, #9183, #8138 ) ;
#3123 = CARTESIAN_POINT ( 'NONE',  ( -1025.296800000965050, 108.9225844456047696, -103.3307627799635782 ) ) ;
#3124 = CARTESIAN_POINT ( 'NONE',  ( -240.0000000000000000, 12.00000000000001066, -126.4213562373078190 ) ) ;
#3125 = CARTESIAN_POINT ( 'NONE',  ( 7.500000000000000000, 0.000000000000000000, 0.000000000000000000 ) ) ;
#3126 = AXIS2_PLACEMENT_3D ( 'NONE', #2156, #8706, #8824 ) ;
#3127 = ORIENTED_EDGE ( 'NONE', *, *, #4480, .T. ) ;
#3128 = ORIENTED_EDGE ( 'NONE', *, *, #9702, .F. ) ;
#3129 = CARTESIAN_POINT ( 'NONE',  ( -993.0619804577127070, 103.7129695969639442, -99.57582448894480365 ) ) ;
#3130 = AXIS2_PLACEMENT_3D ( 'NONE', #6989, #1313, #6186 ) ;
#3131 = EDGE_LOOP ( 'NONE', ( #3257, #6840, #1194, #11050 ) ) ;
#3132 = CARTESIAN_POINT ( 'NONE',  ( -1065.000000000005912, 111.6133447792291093, -130.5712005305407217 ) ) ;
#3133 = CARTESIAN_POINT ( 'NONE',  ( -1031.000617048993718, 115.3267894020686697, -136.2353035311981557 ) ) ;
#3134 = CARTESIAN_POINT ( 'NONE',  ( 45.53315400109643463, 12.00000000000000000, -237.8419396193597208 ) ) ;
#3135 = CARTESIAN_POINT ( 'NONE',  ( 20.00000000000000000, 177.7280889209192480, -124.4725468461322890 ) ) ;
#3136 = EDGE_CURVE ( 'NONE', #69, #7247, #2587, .T. ) ;
#3137 = CARTESIAN_POINT ( 'NONE',  ( -1037.348432443215870, 116.4729352038311987, -118.7903414690680961 ) ) ;
#3138 = EDGE_LOOP ( 'NONE', ( #4798, #4827, #11360, #2969 ) ) ;
#3139 = COLOUR_RGB ( '', 0.66274510, 0.83137255, 0.94901961) ;
#3140 = DIRECTION ( 'NONE',  ( 0.000000000000000000, 0.000000000000000000, 1.000000000000000000 ) ) ;
#3141 = DIRECTION ( 'NONE',  ( -0.000000000000000000, -1.000000000000000000, -0.000000000000000000 ) ) ;
#3142 = VECTOR ( 'NONE', #10799, 1000.000000000000000 ) ;
#3143 = PRODUCT_DEFINITION ( 'UNKNOWN', '', #3878, #11351 ) ;
#3144 = CARTESIAN_POINT ( 'NONE',  ( 21.06286287744583774, 178.9509521733696715, -125.7496676813577068 ) ) ;
#3145 = CARTESIAN_POINT ( 'NONE',  ( 4.216865464401061553E-15, 168.0000000000000000, -124.6807709998038405 ) ) ;
#3146 = ORIENTED_EDGE ( 'NONE', *, *, #7457, .T. ) ;
#3147 = FACE_OUTER_BOUND ( 'NONE', #9025, .T. ) ;
#3148 = CARTESIAN_POINT ( 'NONE',  ( -823.7697810748812799, 117.7733807739867871, -124.6807709998041531 ) ) ;
#3149 = DIRECTION ( 'NONE',  ( -0.000000000000000000, 1.000000000000000000, 7.930164461608263644E-17 ) ) ;
#3150 = CARTESIAN_POINT ( 'NONE',  ( -974.3195816561885749, 116.7169707472886842, -141.4553492942758055 ) ) ;
#3151 = B_SPLINE_CURVE_WITH_KNOTS ( 'NONE', 3,
 ( #513, #6897, #10843, #10788, #4238, #8011, #10665, #5037, #2325, #2377, #7072, #3297 ),
 .UNSPECIFIED., .F., .F.,
 ( 4, 2, 2, 2, 2, 4 ),
 ( 0.01304329750449841063, 0.01337875200764213762, 0.01371420651078590625, 0.01438511551707342788, 0.01505602452336094951, 0.01572693352964846941 ),
 .UNSPECIFIED. ) ;
#3152 = CIRCLE ( 'NONE', #11256, 1.000000000000000888 ) ;
#3153 = DIRECTION ( 'NONE',  ( 0.000000000000000000, 0.000000000000000000, 1.000000000000000000 ) ) ;
#3154 = ORIENTED_EDGE ( 'NONE', *, *, #8749, .T. ) ;
#3155 = EDGE_CURVE ( 'NONE', #7478, #12001, #7190, .T. ) ;
#3156 = VERTEX_POINT ( 'NONE', #11062 ) ;
#3157 = DIRECTION ( 'NONE',  ( 8.163404592832031500E-17, -1.000000000000000000, 0.000000000000000000 ) ) ;
#3158 = CARTESIAN_POINT ( 'NONE',  ( -1048.040919118598822, 50.77060569800413248, -146.0307792196448986 ) ) ;
#3159 = CARTESIAN_POINT ( 'NONE',  ( -374.6390623088777829, 89.10776330631169628, -153.5629775697134392 ) ) ;
#3160 = DIRECTION ( 'NONE',  ( 2.040851148208007875E-17, -1.000000000000000000, -0.000000000000000000 ) ) ;
#3161 = CARTESIAN_POINT ( 'NONE',  ( -370.9210819444880940, 58.45107545929887749, -111.3902275226565024 ) ) ;
#3162 = CARTESIAN_POINT ( 'NONE',  ( -828.7970580965601357, 78.02475450683051861, -94.74435982432032688 ) ) ;
#3163 = VERTEX_POINT ( 'NONE', #812 ) ;
#3164 = CARTESIAN_POINT ( 'NONE',  ( -1025.806732200655688, 55.05754055295027172, -136.2353035311988663 ) ) ;
#3165 = ORIENTED_EDGE ( 'NONE', *, *, #3593, .F. ) ;
#3166 = CARTESIAN_POINT ( 'NONE',  ( -1021.637154595298057, 53.81063926482157456, -122.7172756069792285 ) ) ;
#3167 = CARTESIAN_POINT ( 'NONE',  ( -19.99999999999988276, 177.7282845042021791, -124.4700813638023931 ) ) ;
#3168 = CARTESIAN_POINT ( 'NONE',  ( -976.1667687410277949, 38.51511931708004965, -136.2353035311986957 ) ) ;
#3169 = EDGE_LOOP ( 'NONE', ( #8629, #5837, #5953, #4964 ) ) ;
#3170 = CARTESIAN_POINT ( 'NONE',  ( -369.8915433453782953, 55.74834749765059172, -122.7099038825884065 ) ) ;
#3171 = FACE_OUTER_BOUND ( 'NONE', #7700, .T. ) ;
#3172 = DIRECTION ( 'NONE',  ( 0.000000000000000000, 1.000000000000000000, 0.000000000000000000 ) ) ;
#3173 = EDGE_LOOP ( 'NONE', ( #6073, #498, #10667, #6357 ) ) ;
#3174 = VECTOR ( 'NONE', #8869, 1000.000000000000000 ) ;
#3175 = ORIENTED_EDGE ( 'NONE', *, *, #2837, .T. ) ;
#3176 = CARTESIAN_POINT ( 'NONE',  ( -1057.832023714520119, 42.29985473022490794, -126.6442663926294330 ) ) ;
#3177 = CYLINDRICAL_SURFACE ( 'NONE', #2646, 7.500000000000007105 ) ;
#3178 = DIRECTION ( 'NONE',  ( 0.000000000000000000, 1.000000000000000000, 0.000000000000000000 ) ) ;
#3179 = CARTESIAN_POINT ( 'NONE',  ( -926.9570750291553622, 111.1083136274928620, -99.57582448894491733 ) ) ;
#3180 = LINE ( 'NONE', #5271, #7532 ) ;
#3181 = EDGE_CURVE ( 'NONE', #5780, #11075, #10198, .T. ) ;
#3182 = ORIENTED_EDGE ( 'NONE', *, *, #8229, .F. ) ;
#3183 = ADVANCED_FACE ( 'NONE', ( #2720 ), #8298, .F. ) ;
#3184 = ORIENTED_EDGE ( 'NONE', *, *, #321, .T. ) ;
#3185 = CARTESIAN_POINT ( 'NONE',  ( -994.1998135634719347, 88.30642396300639518, -95.06748246948001224 ) ) ;
#3186 = VERTEX_POINT ( 'NONE', #5560 ) ;
#3187 = CARTESIAN_POINT ( 'NONE',  ( -1024.722591077094876, 118.3980260646368379, -130.5712005305404944 ) ) ;
#3188 = CARTESIAN_POINT ( 'NONE',  ( -1013.875822516558969, 120.2710389253236940, -126.6442663926291061 ) ) ;
#3189 = CARTESIAN_POINT ( 'NONE',  ( 3.133148353965215262E-13, 0.000000000000000000, -103.9213562373094959 ) ) ;
#3190 = DIRECTION ( 'NONE',  ( -0.000000000000000000, -1.000000000000000000, -0.000000000000000000 ) ) ;
#3191 = AXIS2_PLACEMENT_3D ( 'NONE', #8656, #1179, #5048 ) ;
#3192 = AXIS2_PLACEMENT_3D ( 'NONE', #239, #4025, #11568 ) ;
#3193 = CARTESIAN_POINT ( 'NONE',  ( -1045.967528061859412, 112.8272211019270230, -113.1262384684098663 ) ) ;
#3194 = CARTESIAN_POINT ( 'NONE',  ( -828.8285638327240576, 78.67432280806576728, -94.77914401073080342 ) ) ;
#3195 = CARTESIAN_POINT ( 'NONE',  ( -828.8208027856991293, 78.99693817035492316, -104.9068376039972321 ) ) ;
#3196 = CARTESIAN_POINT ( 'NONE',  ( -928.4368846968633306, 59.55532739646334051, -124.6807709998041105 ) ) ;
#3197 = EDGE_CURVE ( 'NONE', #505, #5440, #6157, .T. ) ;
#3198 =( NAMED_UNIT ( * ) PLANE_ANGLE_UNIT ( ) SI_UNIT ( $, .RADIAN. ) );
#3199 = EDGE_LOOP ( 'NONE', ( #3778, #1566 ) ) ;
#3200 = DIRECTION ( 'NONE',  ( 0.000000000000000000, 0.000000000000000000, 1.000000000000000000 ) ) ;
#3201 = DIRECTION ( 'NONE',  ( 1.000000000000000000, 4.236366511936864528E-16, 3.037002292462560327E-31 ) ) ;
#3202 = VECTOR ( 'NONE', #9556, 1000.000000000000000 ) ;
#3203 = EDGE_CURVE ( 'NONE', #2309, #6181, #11308, .T. ) ;
#3204 = DIRECTION ( 'NONE',  ( 0.000000000000000000, 1.000000000000000000, 0.000000000000000000 ) ) ;
#3205 = CARTESIAN_POINT ( 'NONE',  ( -951.9057582426059980, 113.9552214607316216, -146.0307792196438754 ) ) ;
#3206 = DIRECTION ( 'NONE',  ( 0.000000000000000000, 0.000000000000000000, 1.000000000000000000 ) ) ;
#3207 = VERTEX_POINT ( 'NONE', #5427 ) ;
#3208 = CARTESIAN_POINT ( 'NONE',  ( -379.4971532347070706, 62.56077224799714998, -129.4206578983209113 ) ) ;
#3209 = CARTESIAN_POINT ( 'NONE',  ( -995.4135022096103285, 71.70161378084171133, -154.2940595301282656 ) ) ;
#3210 = CARTESIAN_POINT ( 'NONE',  ( -374.3221583053840504, 91.81152812351068349, -152.5535231342899749 ) ) ;
#3211 = CARTESIAN_POINT ( 'NONE',  ( 7.750278301654327006E-16, 197.0000000000000000, -124.6807709998038405 ) ) ;
#3212 = EDGE_CURVE ( 'NONE', #759, #11584, #5704, .T. ) ;
#3213 = CARTESIAN_POINT ( 'NONE',  ( -823.1773471095956438, 73.70622229620707344, -94.71566886200753288 ) ) ;
#3214 = AXIS2_PLACEMENT_3D ( 'NONE', #719, #12168, #7335 ) ;
#3216 = EDGE_CURVE ( 'NONE', #10417, #11203, #6289, .T. ) ;
#3215 = CARTESIAN_POINT ( 'NONE',  ( -823.8285638327242850, 78.67432280806536937, -90.68077099980378364 ) ) ;
#3217 = DIRECTION ( 'NONE',  ( 0.000000000000000000, 0.000000000000000000, 1.000000000000000000 ) ) ;
#3218 = ORIENTED_EDGE ( 'NONE', *, *, #5033, .T. ) ;
#3219 = CARTESIAN_POINT ( 'NONE',  ( -1038.506348936321501, 51.71309463382193883, -146.0307792196451260 ) ) ;
#3220 = ORIENTED_EDGE ( 'NONE', *, *, #1457, .T. ) ;
#3221 = DIRECTION ( 'NONE',  ( 0.000000000000000000, 0.000000000000000000, 1.000000000000000000 ) ) ;
#3222 = CIRCLE ( 'NONE', #8943, 7.500000000000013323 ) ;
#3223 = CARTESIAN_POINT ( 'NONE',  ( -1057.693846703447207, 44.87596864925360052, -113.1262384684097100 ) ) ;
#3224 = CARTESIAN_POINT ( 'NONE',  ( -828.8285638327240576, 78.67432280806576728, -94.77914401073080342 ) ) ;
#3225 = CARTESIAN_POINT ( 'NONE',  ( -380.1314642070832406, 100.3266783612533288, -116.5856617868500962 ) ) ;
#3226 = DIRECTION ( 'NONE',  ( 0.000000000000000000, 0.000000000000000000, -1.000000000000000000 ) ) ;
#3227 = ORIENTED_EDGE ( 'NONE', *, *, #7371, .F. ) ;
#3228 = ADVANCED_BREP_SHAPE_REPRESENTATION ( '', ( #8194, #11957 ), #6826 ) ;
#3229 = ORIENTED_EDGE ( 'NONE', *, *, #1166, .T. ) ;
#3230 = CARTESIAN_POINT ( 'NONE',  ( -1014.107508992752514, 52.59077491224128664, -118.7903414690682951 ) ) ;
#3231 = CIRCLE ( 'NONE', #6397, 7.500000000000007105 ) ;
#3232 = AXIS2_PLACEMENT_3D ( 'NONE', #11313, #10567, #3892 ) ;
#3233 = CARTESIAN_POINT ( 'NONE',  ( -127.4999999999999716, -9.213203435596451385, -126.4213562373086575 ) ) ;
#3234 = UNCERTAINTY_MEASURE_WITH_UNIT (LENGTH_MEASURE( 1.000000000000000082E-05 ), #2382, 'distance_accuracy_value', 'NONE');
#3235 = DIRECTION ( 'NONE',  ( -1.000000000000000000, 0.000000000000000000, 0.000000000000000000 ) ) ;
#3236 = CARTESIAN_POINT ( 'NONE',  ( -1014.632462699974781, 105.5176738732103132, -99.57582448894522997 ) ) ;
#3237 = DIRECTION ( 'NONE',  ( -1.000000000000000000, 0.000000000000000000, 0.000000000000000000 ) ) ;
#3238 = CIRCLE ( 'NONE', #2448, 35.00000000000000711 ) ;
#3239 = ORIENTED_EDGE ( 'NONE', *, *, #3405, .F. ) ;
#3240 = VECTOR ( 'NONE', #7946, 1000.000000000000000 ) ;
#3241 = ORIENTED_EDGE ( 'NONE', *, *, #904, .F. ) ;
#3242 = CARTESIAN_POINT ( 'NONE',  ( -974.6181169426257611, 104.3135445892214506, -99.57582448894483207 ) ) ;
#3243 = DIRECTION ( 'NONE',  ( 0.000000000000000000, 0.000000000000000000, -1.000000000000000000 ) ) ;
#3244 = CARTESIAN_POINT ( 'NONE',  ( -954.0688428831344936, 124.4732772249357282, -130.5712005305405796 ) ) ;
#3245 = CARTESIAN_POINT ( 'NONE',  ( -823.7697810748812799, 117.7733807739867871, -124.6807709998041531 ) ) ;
#3246 = LINE ( 'NONE', #2333, #11941 ) ;
#3247 = EDGE_CURVE ( 'NONE', #1219, #5163, #7881, .T. ) ;
#3248 = VECTOR ( 'NONE', #11446, 1000.000000000000000 ) ;
#3249 = LINE ( 'NONE', #350, #9319 ) ;
#3250 = VECTOR ( 'NONE', #10946, 1000.000000000000000 ) ;
#3251 = DIRECTION ( 'NONE',  ( 1.000000000000000000, 1.486905836551548832E-16, -0.000000000000000000 ) ) ;
#3252 = CARTESIAN_POINT ( 'NONE',  ( -20.00000000000014211, 182.6816575896965844, -124.4897194826051816 ) ) ;
#3253 = FACE_BOUND ( 'NONE', #4939, .T. ) ;
#3254 = CARTESIAN_POINT ( 'NONE',  ( 0.000000000000000000, -7.794228634059949812, -4.499999999999995559 ) ) ;
#3255 = STYLED_ITEM ( 'NONE', ( #4685 ), #12079 ) ;
#3256 = FACE_BOUND ( 'NONE', #9685, .T. ) ;
#3257 = ORIENTED_EDGE ( 'NONE', *, *, #4672, .F. ) ;
#3258 = DIRECTION ( 'NONE',  ( 0.000000000000000000, 0.000000000000000000, -1.000000000000000000 ) ) ;
#3259 = DIRECTION ( 'NONE',  ( -0.000000000000000000, 0.8660254037844389297, 0.4999999999999995004 ) ) ;
#3260 = DIRECTION ( 'NONE',  ( -0.000000000000000000, -1.000000000000000000, -0.000000000000000000 ) ) ;
#3261 = DIRECTION ( 'NONE',  ( -0.000000000000000000, 1.000000000000000000, -0.000000000000000000 ) ) ;
#3262 = EDGE_CURVE ( 'NONE', #233, #9732, #876, .T. ) ;
#3263 = FACE_OUTER_BOUND ( 'NONE', #6900, .T. ) ;
#3264 = EDGE_CURVE ( 'NONE', #10273, #8366, #11823, .T. ) ;
#3265 = ORIENTED_EDGE ( 'NONE', *, *, #1613, .F. ) ;
#3266 = ORIENTED_EDGE ( 'NONE', *, *, #10375, .F. ) ;
#3267 = CARTESIAN_POINT ( 'NONE',  ( 35.00000000000000000, 152.0000000000000000, 190.3192290001959748 ) ) ;
#3268 = CYLINDRICAL_SURFACE ( 'NONE', #7817, 7.500000000000007105 ) ;
#3269 = ORIENTED_EDGE ( 'NONE', *, *, #5649, .T. ) ;
#3270 = EDGE_CURVE ( 'NONE', #9028, #7054, #10825, .T. ) ;
#3271 = DIRECTION ( 'NONE',  ( 0.000000000000000000, 0.000000000000000000, -1.000000000000000000 ) ) ;
#3272 = CARTESIAN_POINT ( 'NONE',  ( 57.50000000000000000, 0.000000000000000000, 0.000000000000000000 ) ) ;
#3273 = CARTESIAN_POINT ( 'NONE',  ( 0.000000000000000000, -492.9999999999998863, -126.4213562373094959 ) ) ;
#3274 = PRESENTATION_STYLE_ASSIGNMENT (( #11577 ) ) ;
#3275 = CYLINDRICAL_SURFACE ( 'NONE', #1360, 7.500000000000007105 ) ;
#3276 = EDGE_LOOP ( 'NONE', ( #1213, #1176, #9743, #11116 ) ) ;
#3277 = CARTESIAN_POINT ( 'NONE',  ( -1065.000000000001364, 65.22545431197576704, -149.7857175106635168 ) ) ;
#3278 = CIRCLE ( 'NONE', #10196, 7.500000000000007105 ) ;
#3279 = ORIENTED_EDGE ( 'NONE', *, *, #6743, .F. ) ;
#3280 = ORIENTED_EDGE ( 'NONE', *, *, #9725, .T. ) ;
#3281 = CARTESIAN_POINT ( 'NONE',  ( -210.0000000000000000, 139.9999999999999716, -126.4213562373080180 ) ) ;
#3282 = EDGE_CURVE ( 'NONE', #7020, #10331, #8231, .T. ) ;
#3283 = CARTESIAN_POINT ( 'NONE',  ( -1017.027421246622112, 56.01181809833683900, -113.1262384684095537 ) ) ;
#3284 = CARTESIAN_POINT ( 'NONE',  ( 8.099999999999999645, 8.082668874372530033E-16, 6.599999999999998757 ) ) ;
#3285 = CIRCLE ( 'NONE', #10398, 7.500000000000007105 ) ;
#3286 = CARTESIAN_POINT ( 'NONE',  ( -828.8285638327250808, 79.00071959000507604, -94.79793468034198156 ) ) ;
#3287 = DIRECTION ( 'NONE',  ( 0.000000000000000000, 1.000000000000000000, -0.000000000000000000 ) ) ;
#3288 = VERTEX_POINT ( 'NONE', #9398 ) ;
#3289 = ADVANCED_FACE ( 'NONE', ( #934 ), #4706, .F. ) ;
#3290 = VERTEX_POINT ( 'NONE', #8657 ) ;
#3291 = CARTESIAN_POINT ( 'NONE',  ( -8.499999999999998224, 166.0000000000000000, -124.6807709998038405 ) ) ;
#3292 = AXIS2_PLACEMENT_3D ( 'NONE', #6416, #3435, #7222 ) ;
#3293 = VECTOR ( 'NONE', #8127, 1000.000000000000000 ) ;
#3294 = CARTESIAN_POINT ( 'NONE',  ( -27.99999999999999645, -492.9999999999998863, -27.99999999999999645 ) ) ;
#3295 = EDGE_CURVE ( 'NONE', #5214, #2170, #3315, .T. ) ;
#3296 = CARTESIAN_POINT ( 'NONE',  ( -821.6815100408621220, 89.78153722040228502, -96.78565065507908116 ) ) ;
#3297 = CARTESIAN_POINT ( 'NONE',  ( -19.87519864879851994, 178.8871479037923393, -126.9115732480538838 ) ) ;
#3298 = EDGE_LOOP ( 'NONE', ( #1885, #8268, #8263, #10866 ) ) ;
#3299 = DIRECTION ( 'NONE',  ( -0.000000000000000000, 1.000000000000000000, 7.930164461608263644E-17 ) ) ;
#3300 =( NAMED_UNIT ( * ) SI_UNIT ( $, .STERADIAN. ) SOLID_ANGLE_UNIT ( ) );
#3301 = ORIENTED_EDGE ( 'NONE', *, *, #6516, .F. ) ;
#3302 = AXIS2_PLACEMENT_3D ( 'NONE', #9, #11275, #8614 ) ;
#3303 = DIRECTION ( 'NONE',  ( 0.000000000000000000, -1.000000000000000000, 0.000000000000000000 ) ) ;
#3304 = CYLINDRICAL_SURFACE ( 'NONE', #3653, 7.500000000000007105 ) ;
#3305 = ORIENTED_EDGE ( 'NONE', *, *, #1613, .T. ) ;
#3306 = DIRECTION ( 'NONE',  ( 1.000000000000000000, 0.000000000000000000, 0.000000000000000000 ) ) ;
#3307 = DIRECTION ( 'NONE',  ( -1.000000000000000000, 0.000000000000000000, 0.000000000000000000 ) ) ;
#3308 = CARTESIAN_POINT ( 'NONE',  ( -21.04833203300971789, 181.6140747827068935, -125.4344175246748563 ) ) ;
#3309 = CARTESIAN_POINT ( 'NONE',  ( -35.00000000000000000, 81.99999999999998579, 190.3192290001959748 ) ) ;
#3310 = CIRCLE ( 'NONE', #548, 7.500000000000007994 ) ;
#3311 = DIRECTION ( 'NONE',  ( -0.000000000000000000, -1.000000000000000000, -0.000000000000000000 ) ) ;
#3312 = CARTESIAN_POINT ( 'NONE',  ( -826.8820017808986904, 82.64709913614485970, -104.6904163631600824 ) ) ;
#3313 = CARTESIAN_POINT ( 'NONE',  ( -379.1619848709567009, 61.99999999999992184, -124.1323191136051776 ) ) ;
#3314 = CARTESIAN_POINT ( 'NONE',  ( -819.4886053768613010, 81.17856470051358997, -94.91880207566623540 ) ) ;
#3315 = CIRCLE ( 'NONE', #1965, 7.500000000000007105 ) ;
#3316 = ORIENTED_EDGE ( 'NONE', *, *, #5104, .F. ) ;
#3317 = CARTESIAN_POINT ( 'NONE',  ( 30.00000000000000000, -6.000000000000000000, 30.00000000000000000 ) ) ;
#3318 = CARTESIAN_POINT ( 'NONE',  ( -823.7697810748826441, 117.7733807739869292, -126.6442663926291914 ) ) ;
#3319 = VECTOR ( 'NONE', #620, 1000.000000000000000 ) ;
#3320 = CARTESIAN_POINT ( 'NONE',  ( 1.249585401188644101E-12, -6.000000000000005329, -6.421356237309495008 ) ) ;
#3321 = CARTESIAN_POINT ( 'NONE',  ( -45.53315400109751465, 12.00000000000000000, -245.3419396193594650 ) ) ;
#3322 = DIRECTION ( 'NONE',  ( 0.000000000000000000, 0.000000000000000000, -1.000000000000000000 ) ) ;
#3323 = ORIENTED_EDGE ( 'NONE', *, *, #9548, .F. ) ;
#3324 = STYLED_ITEM ( 'NONE', ( #9337 ), #3758 ) ;
#3325 = ORIENTED_EDGE ( 'NONE', *, *, #11937, .T. ) ;
#3326 = CARTESIAN_POINT ( 'NONE',  ( 19.96127628319862879, 179.8817259792408549, -123.2228033267029019 ) ) ;
#3327 = CARTESIAN_POINT ( 'NONE',  ( -381.0129949838454877, 65.36129575118090429, -135.8392840662656056 ) ) ;
#3328 = CARTESIAN_POINT ( 'NONE',  ( -1031.956718292102323, 74.21439239895576634, -154.2940595301282656 ) ) ;
#3329 = CARTESIAN_POINT ( 'NONE',  ( -825.4626643026906549, 73.93730723265454685, -142.9841191000405729 ) ) ;
#3330 = EDGE_CURVE ( 'NONE', #2282, #9776, #3890, .T. ) ;
#3331 = CARTESIAN_POINT ( 'NONE',  ( -371.1973815542190778, 104.7660296280457715, -139.6871427982646026 ) ) ;
#3332 = DIRECTION ( 'NONE',  ( -1.186840563529527301E-16, 1.000000000000000000, -0.000000000000000000 ) ) ;
#3333 = CARTESIAN_POINT ( 'NONE',  ( -35.00000000000000000, 12.00000000000002309, -159.6807709998040252 ) ) ;
#3334 = EDGE_CURVE ( 'NONE', #11656, #6719, #12016, .T. ) ;
#3335 = PRESENTATION_STYLE_ASSIGNMENT (( #558 ) ) ;
#3336 = AXIS2_PLACEMENT_3D ( 'NONE', #7880, #10773, #9848 ) ;
#3337 = VECTOR ( 'NONE', #5544, 1000.000000000000000 ) ;
#3338 = ORIENTED_EDGE ( 'NONE', *, *, #6229, .T. ) ;
#3339 = CARTESIAN_POINT ( 'NONE',  ( -975.7625022073049195, 55.15120678236734619, -149.7857175106636589 ) ) ;
#3340 = ORIENTED_EDGE ( 'NONE', *, *, #120, .T. ) ;
#3341 = ORIENTED_EDGE ( 'NONE', *, *, #6226, .F. ) ;
#3342 = DIRECTION ( 'NONE',  ( -0.000000000000000000, 1.000000000000000000, -0.000000000000000000 ) ) ;
#3343 = CARTESIAN_POINT ( 'NONE',  ( 28.00000000000000000, -492.9999999999998863, -27.99999999999999645 ) ) ;
#3344 = VERTEX_POINT ( 'NONE', #9633 ) ;
#3345 = LINE ( 'NONE', #1326, #11505 ) ;
#3346 = ORIENTED_EDGE ( 'NONE', *, *, #2837, .F. ) ;
#3347 = ORIENTED_EDGE ( 'NONE', *, *, #6546, .T. ) ;
#3348 = EDGE_CURVE ( 'NONE', #2194, #8074, #49, .T. ) ;
#3349 = CARTESIAN_POINT ( 'NONE',  ( -21.06729583384051097, 179.4139655881280078, -126.1965993184190040 ) ) ;
#3350 = ADVANCED_FACE ( 'NONE', ( #5926 ), #7479, .T. ) ;
#3351 = CARTESIAN_POINT ( 'NONE',  ( -1022.719357623492556, 104.5170332807322922, -99.57582448894488891 ) ) ;
#3352 = CARTESIAN_POINT ( 'NONE',  ( -35.00000000000000000, 12.00000000000001954, -124.6807709998040110 ) ) ;
#3353 = ORIENTED_EDGE ( 'NONE', *, *, #3655, .F. ) ;
#3354 = CARTESIAN_POINT ( 'NONE',  ( 6.899999999999999467, 5.196152422706624030, -9.000000000000000000 ) ) ;
#3355 = CARTESIAN_POINT ( 'NONE',  ( -374.9690483538964259, 84.66840056888385391, -104.8435496553661181 ) ) ;
#3356 = EDGE_LOOP ( 'NONE', ( #11380, #3855 ) ) ;
#3357 = CARTESIAN_POINT ( 'NONE',  ( -20.71964524312745581, 180.0381522043864777, -123.3053720114591130 ) ) ;
#3358 = DIRECTION ( 'NONE',  ( -1.000000000000000000, 0.000000000000000000, 0.000000000000000000 ) ) ;
#3359 = ORIENTED_EDGE ( 'NONE', *, *, #1844, .F. ) ;
#3360 = CARTESIAN_POINT ( 'NONE',  ( -828.8285638327247398, 79.00071603608273563, -154.5636075238658691 ) ) ;
#3361 = CARTESIAN_POINT ( 'NONE',  ( -975.3893330992572146, 71.12659035875115876, -95.06748246948035330 ) ) ;
#3362 = EDGE_CURVE ( 'NONE', #9776, #338, #367, .T. ) ;
#3363 = CARTESIAN_POINT ( 'NONE',  ( 20.00000000000000000, 182.6968134406613160, -124.6807709998155076 ) ) ;
#3364 = CARTESIAN_POINT ( 'NONE',  ( -20.87185099990339410, 181.4830870518408972, -123.9928801481976564 ) ) ;
#3365 = CYLINDRICAL_SURFACE ( 'NONE', #412, 8.999999999999998224 ) ;
#3366 = CARTESIAN_POINT ( 'NONE',  ( -818.8285638327240576, 78.67432280806558254, -104.9592124606052295 ) ) ;
#3367 = AXIS2_PLACEMENT_3D ( 'NONE', #11658, #6029, #9911 ) ;
#3368 = FACE_BOUND ( 'NONE', #2347, .T. ) ;
#3369 = DIRECTION ( 'NONE',  ( 0.000000000000000000, 0.000000000000000000, 1.000000000000000000 ) ) ;
#3370 = ORIENTED_EDGE ( 'NONE', *, *, #4133, .T. ) ;
#3371 = CARTESIAN_POINT ( 'NONE',  ( 0.000000000000000000, 0.000000000000000000, 8.999999999999998224 ) ) ;
#3372 = CARTESIAN_POINT ( 'NONE',  ( -852.8175266017512968, 121.6828083272127685, -122.7172756069790438 ) ) ;
#3373 = DIRECTION ( 'NONE',  ( 0.7071067811865477948, 0.000000000000000000, 0.7071067811865473507 ) ) ;
#3374 = CYLINDRICAL_SURFACE ( 'NONE', #11416, 7.500000000000007105 ) ;
#3375 = DIRECTION ( 'NONE',  ( -0.000000000000000000, 1.000000000000000000, -0.000000000000000000 ) ) ;
#3376 = AXIS2_PLACEMENT_3D ( 'NONE', #4147, #5182, #6056 ) ;
#3377 = CARTESIAN_POINT ( 'NONE',  ( -925.0000000000000000, 81.99999999999988631, -124.6807709998038405 ) ) ;
#3378 = ORIENTED_EDGE ( 'NONE', *, *, #1523, .F. ) ;
#3379 = CARTESIAN_POINT ( 'NONE',  ( -19.89107406457440774, 179.2763954864628602, -122.5941855233586466 ) ) ;
#3380 = CARTESIAN_POINT ( 'NONE',  ( 154.5043356068769071, 12.00000000000000000, -94.56666130601712439 ) ) ;
#3381 = CARTESIAN_POINT ( 'NONE',  ( -1015.825132819589953, 80.44428838836770979, -154.2940595301284645 ) ) ;
#3382 = CARTESIAN_POINT ( 'NONE',  ( -379.3681879713551552, 101.6576152188101503, -128.5919495273215603 ) ) ;
#3383 = VECTOR ( 'NONE', #4203, 1000.000000000000000 ) ;
#3384 = DIRECTION ( 'NONE',  ( 0.000000000000000000, 0.000000000000000000, 1.000000000000000000 ) ) ;
#3385 = CARTESIAN_POINT ( 'NONE',  ( -119.9999999999999858, -9.213203435596451385, -126.4213562373086575 ) ) ;
#3386 = CARTESIAN_POINT ( 'NONE',  ( 7.500000000000009770, 139.9999999999999716, -126.4213562373094959 ) ) ;
#3387 = DIRECTION ( 'NONE',  ( -0.000000000000000000, -1.000000000000000000, -0.000000000000000000 ) ) ;
#3388 = DIRECTION ( 'NONE',  ( 0.000000000000000000, 0.000000000000000000, -1.000000000000000000 ) ) ;
#3389 = ORIENTED_EDGE ( 'NONE', *, *, #5441, .F. ) ;
#3390 = CARTESIAN_POINT ( 'NONE',  ( -795.0000000000071623, 60.65002596136950075, -146.0307792196447565 ) ) ;
#3391 = CIRCLE ( 'NONE', #859, 7.500000000000007105 ) ;
#3392 = ORIENTED_EDGE ( 'NONE', *, *, #5946, .T. ) ;
#3393 = ADVANCED_FACE ( 'NONE', ( #2037, #4871, #9456, #3826, #4934 ), #9578, .T. ) ;
#3394 = DIRECTION ( 'NONE',  ( 0.000000000000000000, 0.000000000000000000, 1.000000000000000000 ) ) ;
#3395 = B_SPLINE_CURVE_WITH_KNOTS ( 'NONE', 3,
 ( #1570, #11890, #6144, #392, #7132, #11720 ),
 .UNSPECIFIED., .F., .F.,
 ( 4, 2, 4 ),
 ( 2.380730968235596737E-07, 0.002629065763328352224, 0.005257893453559881088 ),
 .UNSPECIFIED. ) ;
#3396 = EDGE_LOOP ( 'NONE', ( #10120, #11963, #11935, #1737 ) ) ;
#3397 = CARTESIAN_POINT ( 'NONE',  ( -380.8566067580512708, 98.94424270813378541, -114.0399298516432225 ) ) ;
#3398 = VERTEX_POINT ( 'NONE', #1118 ) ;
#3399 = DIRECTION ( 'NONE',  ( -1.224646799147353207E-16, -1.453460497224676649E-32, 1.000000000000000000 ) ) ;
#3400 = ORIENTED_EDGE ( 'NONE', *, *, #2069, .T. ) ;
#3401 = FACE_OUTER_BOUND ( 'NONE', #4385, .T. ) ;
#3402 = DIRECTION ( 'NONE',  ( 0.000000000000000000, -1.000000000000000000, 0.000000000000000000 ) ) ;
#3403 = AXIS2_PLACEMENT_3D ( 'NONE', #8452, #8557, #9363 ) ;
#3404 = CYLINDRICAL_SURFACE ( 'NONE', #7837, 7.500000000000007105 ) ;
#3405 = EDGE_CURVE ( 'NONE', #6750, #6717, #5858, .T. ) ;
#3406 = CARTESIAN_POINT ( 'NONE',  ( -1047.392513188126713, 70.23666496464434772, -95.06748246948035330 ) ) ;
#3407 = CARTESIAN_POINT ( 'NONE',  ( 1.387778780781445676E-14, -6.000000000000000000, 133.9213562373095101 ) ) ;
#3408 = CARTESIAN_POINT ( 'NONE',  ( -120.8820948793972434, 12.00000000000000000, -186.6989091883324363 ) ) ;
#3409 = DIRECTION ( 'NONE',  ( -8.163404592832031500E-17, 1.000000000000000000, 0.000000000000000000 ) ) ;
#3410 = CARTESIAN_POINT ( 'NONE',  ( -795.0000000000048885, 52.00000000000024158, -124.6807709998040821 ) ) ;
#3411 = CARTESIAN_POINT ( 'NONE',  ( -375.0005549305242312, 83.05317239051150580, -104.6789509088160628 ) ) ;
#3412 = ORIENTED_EDGE ( 'NONE', *, *, #1545, .T. ) ;
#3413 = AXIS2_PLACEMENT_3D ( 'NONE', #4372, #5546, #6594 ) ;
#3414 = CARTESIAN_POINT ( 'NONE',  ( 1.387778780781445676E-14, -492.9999999999998863, 126.4213562373094959 ) ) ;
#3415 = ADVANCED_FACE ( 'NONE', ( #4015 ), #11558, .F. ) ;
#3416 = AXIS2_PLACEMENT_3D ( 'NONE', #6745, #10582, #8731 ) ;
#3417 = CARTESIAN_POINT ( 'NONE',  ( 154.5043356068769071, 0.000000000000000000, -109.5666613060171670 ) ) ;
#3418 = VERTEX_POINT ( 'NONE', #7782 ) ;
#3419 = CARTESIAN_POINT ( 'NONE',  ( -825.1280624195762812, 83.51352241364627105, -154.1197328629658045 ) ) ;
#3420 = CARTESIAN_POINT ( 'NONE',  ( -1047.392513188126713, 70.23666496464434772, -95.06748246948035330 ) ) ;
#3421 = CARTESIAN_POINT ( 'NONE',  ( 0.3570196857253478684, 9.540868182094902394, 1.474731560294324728 ) ) ;
#3422 = B_SPLINE_CURVE_WITH_KNOTS ( 'NONE', 3,
 ( #9822, #10810, #6121, #364, #6980, #7103, #1362, #2400, #4201, #7040, #1421, #1479, #4023, #7348, #11121, #8224, #11861, #4448, #2643, #11984, #6422, #5722, #7414, #5420, #1537, #5295 ),
 .UNSPECIFIED., .F., .F.,
 ( 4, 2, 2, 2, 2, 2, 2, 2, 2, 2, 2, 2, 4 ),
 ( 0.04496985353261317292, 0.04715854719908585402, 0.04934724086555854206, 0.05372462819850394589, 0.05591332186497667556, 0.05810201553144939135, 0.06247940286439480212, 0.06466809653086749710, 0.06685679019734019901, 0.07123417753028561672, 0.07342287119675831863, 0.07561156486323100667, 0.07998895219617635499 ),
 .UNSPECIFIED. ) ;
#3423 = DIRECTION ( 'NONE',  ( -3.061276722312011504E-17, 1.000000000000000000, 0.000000000000000000 ) ) ;
#3424 = CARTESIAN_POINT ( 'NONE',  ( -951.4198147059590838, 125.0824040815807194, -126.6442663926291345 ) ) ;
#3425 = CYLINDRICAL_SURFACE ( 'NONE', #3780, 7.500000000000007105 ) ;
#3426 = VECTOR ( 'NONE', #7420, 999.9999999999998863 ) ;
#3427 = CIRCLE ( 'NONE', #7996, 7.500000000000007105 ) ;
#3428 = CARTESIAN_POINT ( 'NONE',  ( 6.257111856936825515E-13, 0.000000000000000000, -73.92135623730949590 ) ) ;
#3429 = CARTESIAN_POINT ( 'NONE',  ( 0.000000000000000000, 152.0000000000000000, -124.6807709998038405 ) ) ;
#3430 = ADVANCED_FACE ( 'NONE', ( #6672 ), #168, .F. ) ;
#3431 = CARTESIAN_POINT ( 'NONE',  ( -823.5000624989246489, 83.67424195610568916, -104.7509713550764872 ) ) ;
#3432 = CARTESIAN_POINT ( 'NONE',  ( -976.2517683711889731, 35.25052392388816713, -124.6807709998040394 ) ) ;
#3433 = CARTESIAN_POINT ( 'NONE',  ( -818.9957115137622168, 77.38185006597193194, -154.6675616934836057 ) ) ;
#3434 = VERTEX_POINT ( 'NONE', #3084 ) ;
#3435 = DIRECTION ( 'NONE',  ( -1.000000000000000000, -0.000000000000000000, -0.000000000000000000 ) ) ;
#3436 = CARTESIAN_POINT ( 'NONE',  ( -974.1288507787422759, 124.2142274477005657, -124.6807709998040110 ) ) ;
#3437 = ADVANCED_FACE ( 'NONE', ( #2105, #11370, #6857, #8771, #1236 ), #2910, .F. ) ;
#3438 = EDGE_CURVE ( 'NONE', #178, #5809, #2164, .T. ) ;
#3439 = VECTOR ( 'NONE', #4347, 1000.000000000000000 ) ;
#3440 = AXIS2_PLACEMENT_3D ( 'NONE', #4510, #3559, #12128 ) ;
#3441 = CARTESIAN_POINT ( 'NONE',  ( 2.186774452080127126E-12, 12.00000000000000000, 91.07864376269050410 ) ) ;
#3442 = DIRECTION ( 'NONE',  ( 1.186840563529527301E-16, -1.000000000000000000, 0.000000000000000000 ) ) ;
#3443 = CARTESIAN_POINT ( 'NONE',  ( 151.3258811035896656, 0.000000000000000000, -56.13263083939798292 ) ) ;
#3444 = CARTESIAN_POINT ( 'NONE',  ( 19.99747163337677591, 182.7034818914266339, -125.0350401822433497 ) ) ;
#3445 = ORIENTED_EDGE ( 'NONE', *, *, #2302, .T. ) ;
#3446 = ORIENTED_EDGE ( 'NONE', *, *, #2102, .F. ) ;
#3447 = CARTESIAN_POINT ( 'NONE',  ( 20.74743244309822288, 180.7984090500023626, -123.4190994394879937 ) ) ;
#3448 = EDGE_CURVE ( 'NONE', #4344, #2975, #4904, .T. ) ;
#3449 = AXIS2_PLACEMENT_3D ( 'NONE', #7914, #9817, #5175 ) ;
#3450 = CARTESIAN_POINT ( 'NONE',  ( -305.0000000000000568, 81.99999999999995737, -159.6807709998038547 ) ) ;
#3451 = FACE_BOUND ( 'NONE', #10289, .T. ) ;
#3452 = FACE_OUTER_BOUND ( 'NONE', #11635, .T. ) ;
#3453 = DIRECTION ( 'NONE',  ( -0.000000000000000000, 1.000000000000000000, -0.000000000000000000 ) ) ;
#3454 = ORIENTED_EDGE ( 'NONE', *, *, #8431, .T. ) ;
#3455 = CARTESIAN_POINT ( 'NONE',  ( -818.8285638327245124, 78.34431818532443970, -94.72265437454855430 ) ) ;
#3456 = ORIENTED_EDGE ( 'NONE', *, *, #6780, .F. ) ;
#3457 = CARTESIAN_POINT ( 'NONE',  ( -795.0000000000011369, 65.22545431197602284, -149.7857175106635452 ) ) ;
#3458 = ORIENTED_EDGE ( 'NONE', *, *, #1480, .T. ) ;
#3459 = ORIENTED_EDGE ( 'NONE', *, *, #10530, .T. ) ;
#3460 = CARTESIAN_POINT ( 'NONE',  ( -19.97716120749745627, 179.8971463893286398, -126.1313698542638235 ) ) ;
#3461 = ORIENTED_EDGE ( 'NONE', *, *, #1704, .T. ) ;
#3462 = CARTESIAN_POINT ( 'NONE',  ( -371.2910448380831099, 59.51545945449562680, -140.1702109638846423 ) ) ;
#3463 = CARTESIAN_POINT ( 'NONE',  ( 1.387778780781445676E-14, 11.99999999999999645, 126.4213562373094959 ) ) ;
#3464 = DIRECTION ( 'NONE',  ( 0.000000000000000000, 0.000000000000000000, 1.000000000000000000 ) ) ;
#3465 = ORIENTED_EDGE ( 'NONE', *, *, #5532, .T. ) ;
#3466 = CIRCLE ( 'NONE', #6450, 7.500000000000012434 ) ;
#3467 = DIRECTION ( 'NONE',  ( -1.000000000000000000, -1.186840563529527301E-16, 0.000000000000000000 ) ) ;
#3468 = VERTEX_POINT ( 'NONE', #8590 ) ;
#3469 = DIRECTION ( 'NONE',  ( 0.000000000000000000, 0.000000000000000000, 1.000000000000000000 ) ) ;
#3470 = CARTESIAN_POINT ( 'NONE',  ( 30.00000000000000000, -6.000000000000000000, -30.00000000000000000 ) ) ;
#3471 = FACE_OUTER_BOUND ( 'NONE', #5847, .T. ) ;
#3472 = CARTESIAN_POINT ( 'NONE',  ( 9.184850993605161750E-16, 164.0000000000000000, -133.9213562373095101 ) ) ;
#3473 = CIRCLE ( 'NONE', #1915, 7.500000000000007994 ) ;
#3474 = CARTESIAN_POINT ( 'NONE',  ( -1012.828629370415570, 79.69572830938430741, -95.06748246948046699 ) ) ;
#3475 = DIRECTION ( 'NONE',  ( 0.000000000000000000, 1.000000000000000000, 0.000000000000000000 ) ) ;
#3476 = CARTESIAN_POINT ( 'NONE',  ( 0.000000000000000000, 7.347880794884118750E-16, -5.999999999999999112 ) ) ;
#3477 = ORIENTED_EDGE ( 'NONE', *, *, #9611, .F. ) ;
#3478 = CARTESIAN_POINT ( 'NONE',  ( -20.75374193024407887, 179.5597222894005256, -123.4475611661679864 ) ) ;
#3479 = EDGE_CURVE ( 'NONE', #5145, #8436, #902, .T. ) ;
#3480 = DIRECTION ( 'NONE',  ( 0.000000000000000000, 0.000000000000000000, 1.000000000000000000 ) ) ;
#3481 = LINE ( 'NONE', #7267, #1291 ) ;
#3482 = ORIENTED_EDGE ( 'NONE', *, *, #12070, .F. ) ;
#3483 = CARTESIAN_POINT ( 'NONE',  ( -828.5731522051593174, 80.28512761734042158, -154.4691854747994171 ) ) ;
#3485 = EDGE_CURVE ( 'NONE', #8074, #7241, #9042, .T. ) ;
#3484 = CARTESIAN_POINT ( 'NONE',  ( -1020.082665824770629, 80.34198733739781062, -95.06748246948050962 ) ) ;
#3486 = VECTOR ( 'NONE', #2324, 1000.000000000000000 ) ;
#3487 = CARTESIAN_POINT ( 'NONE',  ( -180.0000000000000000, 139.9999999999999716, -126.4213562373082453 ) ) ;
#3488 = DIRECTION ( 'NONE',  ( 0.000000000000000000, 0.000000000000000000, -1.000000000000000000 ) ) ;
#3489 = DIRECTION ( 'NONE',  ( -0.000000000000000000, -0.000000000000000000, 1.000000000000000000 ) ) ;
#3490 = CARTESIAN_POINT ( 'NONE',  ( -828.7963533401342602, 78.01901522663797550, -105.0781937692939607 ) ) ;
#3491 = CARTESIAN_POINT ( 'NONE',  ( -20.84834133081599106, 179.0338598627802753, -123.8893051224479507 ) ) ;
#3492 = CARTESIAN_POINT ( 'NONE',  ( -150.0000000000000000, 12.00000000000001421, -126.4213562373084301 ) ) ;
#3493 = ORIENTED_EDGE ( 'NONE', *, *, #8467, .F. ) ;
#3494 = CARTESIAN_POINT ( 'NONE',  ( -370.2179477426083167, 56.57026616554610854, -117.1538732267712959 ) ) ;
#3495 = ORIENTED_EDGE ( 'NONE', *, *, #4816, .F. ) ;
#3496 = CARTESIAN_POINT ( 'NONE',  ( -13.32222501832919193, 180.2041921146325762, -184.1652315311841051 ) ) ;
#3497 = CARTESIAN_POINT ( 'NONE',  ( -1054.407929976941432, 113.5897173251036207, -118.7903414690678261 ) ) ;
#3498 = CARTESIAN_POINT ( 'NONE',  ( 1.479627290717497352E-14, 0.000000000000000000, 118.9213562373094817 ) ) ;
#3499 = CARTESIAN_POINT ( 'NONE',  ( 1.387778780781445676E-14, 152.0000000000000284, 126.4213562373094959 ) ) ;
#3500 = DIRECTION ( 'NONE',  ( 0.000000000000000000, 0.000000000000000000, 1.000000000000000000 ) ) ;
#3501 = EDGE_CURVE ( 'NONE', #4515, #3716, #1469, .T. ) ;
#3502 = CARTESIAN_POINT ( 'NONE',  ( 21.06462418130824688, 181.3953932437717924, -125.8282119242440871 ) ) ;
#3503 = VERTEX_POINT ( 'NONE', #7969 ) ;
#3504 = ORIENTED_EDGE ( 'NONE', *, *, #5365, .T. ) ;
#3505 = CARTESIAN_POINT ( 'NONE',  ( -19.85143985168299352, 179.2905725846962639, -127.1146981247506744 ) ) ;
#3506 = CARTESIAN_POINT ( 'NONE',  ( -45.53315400109751465, 12.00000000000000000, -237.8419396193594650 ) ) ;
#3507 = CARTESIAN_POINT ( 'NONE',  ( -1025.928429817215147, 97.79385104913471594, -152.5758913445291398 ) ) ;
#3508 = CARTESIAN_POINT ( 'NONE',  ( -827.8145948178575964, 75.63860347950591745, -143.6442145102269592 ) ) ;
#3509 = CIRCLE ( 'NONE', #5292, 8.500000000000003553 ) ;
#3510 = CARTESIAN_POINT ( 'NONE',  ( 0.000000000000000000, -7.794228634059935601, 4.500000000000016875 ) ) ;
#3511 = CARTESIAN_POINT ( 'NONE',  ( -232.4999999999999716, 139.9999999999999716, -126.4213562373078190 ) ) ;
#3512 = CARTESIAN_POINT ( 'NONE',  ( 3.123963502971610252E-13, -6.000000000000005329, -96.42135623730949590 ) ) ;
#3513 = ORIENTED_EDGE ( 'NONE', *, *, #11610, .T. ) ;
#3514 = CYLINDRICAL_SURFACE ( 'NONE', #8967, 7.499999999999978684 ) ;
#3515 = FACE_OUTER_BOUND ( 'NONE', #11111, .T. ) ;
#3516 = SURFACE_SIDE_STYLE ('',( #3574 ) ) ;
#3517 = EDGE_LOOP ( 'NONE', ( #3003, #998, #2416, #8891 ) ) ;
#3518 = CARTESIAN_POINT ( 'NONE',  ( -247.5000000000000000, 139.9999999999999716, -126.4213562373078190 ) ) ;
#3519 = CARTESIAN_POINT ( 'NONE',  ( -1038.283672687649414, 64.16172732404312740, -152.5758913445294240 ) ) ;
#3520 = EDGE_CURVE ( 'NONE', #6950, #4282, #1364, .T. ) ;
#3521 = AXIS2_PLACEMENT_3D ( 'NONE', #11431, #10562, #11624 ) ;
#3522 = B_SPLINE_CURVE_WITH_KNOTS ( 'NONE', 3,
 ( #1520, #10853, #4251, #7668, #3956, #2971, #2270, #6159, #6733, #3363 ),
 .UNSPECIFIED., .F., .F.,
 ( 4, 2, 2, 2, 4 ),
 ( 0.007575694888659623323, 0.008165068094779329502, 0.008754441300899034814, 0.009343814507018741861, 0.009933187713138447172 ),
 .UNSPECIFIED. ) ;
#3523 = VERTEX_POINT ( 'NONE', #3254 ) ;
#3524 = CARTESIAN_POINT ( 'NONE',  ( -19.84415231186486395, 179.4841820921725173, -127.1732901015634951 ) ) ;
#3525 = ORIENTED_EDGE ( 'NONE', *, *, #6062, .T. ) ;
#3526 = CARTESIAN_POINT ( 'NONE',  ( -372.6100443311099752, 62.67118023337630461, -129.8688800426077705 ) ) ;
#3527 = FACE_OUTER_BOUND ( 'NONE', #5714, .T. ) ;
#3528 = EDGE_LOOP ( 'NONE', ( #11057, #11374, #3551 ) ) ;
#3529 = DIRECTION ( 'NONE',  ( 0.000000000000000000, 1.000000000000000000, 6.938893903907169213E-16 ) ) ;
#3530 = DIRECTION ( 'NONE',  ( 0.3117078928809249860, -1.670400663243698742E-14, 0.9501779778103330854 ) ) ;
#3531 = CARTESIAN_POINT ( 'NONE',  ( -1.017710086126041463E-15, 0.4400770685579608599, 9.000000000000000000 ) ) ;
#3532 = CARTESIAN_POINT ( 'NONE',  ( 19.88188653267749118, 178.7826062614507805, -126.8526954990893927 ) ) ;
#3533 = CARTESIAN_POINT ( 'NONE',  ( -902.8257469293350823, 84.21185948885704420, -95.06748246948052383 ) ) ;
#3534 = DIRECTION ( 'NONE',  ( 0.000000000000000000, 0.000000000000000000, 1.000000000000000000 ) ) ;
#3535 = CARTESIAN_POINT ( 'NONE',  ( 4.255174644013695128E-15, 25.00000000000002132, -126.4213562373094959 ) ) ;
#3536 = CARTESIAN_POINT ( 'NONE',  ( -374.5804915919682117, 74.30254460433448571, -95.98273762526655162 ) ) ;
#3537 = ORIENTED_EDGE ( 'NONE', *, *, #2465, .F. ) ;
#3538 = FACE_BOUND ( 'NONE', #9519, .T. ) ;
#3539 = DIRECTION ( 'NONE',  ( 0.000000000000000000, -0.5000000000000009992, -0.8660254037844380415 ) ) ;
#3540 = ORIENTED_EDGE ( 'NONE', *, *, #2286, .F. ) ;
#3541 = CYLINDRICAL_SURFACE ( 'NONE', #9805, 20.00000000000000000 ) ;
#3542 = LINE ( 'NONE', #3681, #2143 ) ;
#3543 = DIRECTION ( 'NONE',  ( -2.081668171172161734E-17, -4.930380657631307143E-31, 1.000000000000000000 ) ) ;
#3544 = CARTESIAN_POINT ( 'NONE',  ( 19.97657674272267769, 180.1017299760444530, -126.1590557403436037 ) ) ;
#3545 = LINE ( 'NONE', #11106, #5160 ) ;
#3546 = ADVANCED_FACE ( 'NONE', ( #5049 ), #7032, .F. ) ;
#3547 = CARTESIAN_POINT ( 'NONE',  ( -826.3665850287318335, 74.35417337301126395, -106.1988918232330832 ) ) ;
#3548 = CARTESIAN_POINT ( 'NONE',  ( -19.97250828649639587, 179.3956025841652888, -123.4200681550201892 ) ) ;
#3549 = CARTESIAN_POINT ( 'NONE',  ( -825.1469620822797424, 73.83976809224682825, -142.9404499552402115 ) ) ;
#3550 = ADVANCED_FACE ( 'NONE', ( #10986 ), #9752, .F. ) ;
#3551 = ORIENTED_EDGE ( 'NONE', *, *, #3602, .T. ) ;
#3552 = CARTESIAN_POINT ( 'NONE',  ( -369.8650217330579153, 55.68315087016564036, -123.9032152127662130 ) ) ;
#3553 = ORIENTED_EDGE ( 'NONE', *, *, #2267, .T. ) ;
#3554 = CARTESIAN_POINT ( 'NONE',  ( -305.0000000000000568, 81.99999999999995737, -89.68077099980384048 ) ) ;
#3555 = CARTESIAN_POINT ( 'NONE',  ( -991.6207251904191935, 122.2801902404845151, -118.7903414690677124 ) ) ;
#3556 = VECTOR ( 'NONE', #8982, 1000.000000000000000 ) ;
#3557 = DIRECTION ( 'NONE',  ( 2.040851148208007875E-17, -1.000000000000000000, -0.000000000000000000 ) ) ;
#3558 = CARTESIAN_POINT ( 'NONE',  ( 6.247927005943220505E-13, 12.00000000000000000, -58.92135623730948879 ) ) ;
#3559 = DIRECTION ( 'NONE',  ( 0.000000000000000000, 1.000000000000000000, 0.000000000000000000 ) ) ;
#3560 = CARTESIAN_POINT ( 'NONE',  ( 19.99933548561055829, 181.6672375346512922, -124.2941161999968926 ) ) ;
#3561 = VERTEX_POINT ( 'NONE', #2341 ) ;
#3562 = ORIENTED_EDGE ( 'NONE', *, *, #12191, .F. ) ;
#3563 = EDGE_CURVE ( 'NONE', #1690, #5876, #6103, .T. ) ;
#3564 = LINE ( 'NONE', #875, #6753 ) ;
#3565 = CARTESIAN_POINT ( 'NONE',  ( 1.387778780781445676E-14, -58.00000000000000711, 133.9213562373095101 ) ) ;
#3566 = CARTESIAN_POINT ( 'NONE',  ( -820.4595805503685142, 72.64106675864371709, -154.8742214401225397 ) ) ;
#3567 = CARTESIAN_POINT ( 'NONE',  ( -379.5458574098431654, 101.3607069150075830, -129.8688049444577928 ) ) ;
#3568 = CARTESIAN_POINT ( 'NONE',  ( -6.251103150736736502E-15, 8.236864015571823572, -3.733333029993796792 ) ) ;
#3569 = CARTESIAN_POINT ( 'NONE',  ( 0.000000000000000000, -58.00000000000000711, -118.9213562373094817 ) ) ;
#3570 = CARTESIAN_POINT ( 'NONE',  ( -903.4746773471192682, 104.0883302344920480, -152.5758913445288272 ) ) ;
#3571 = VERTEX_POINT ( 'NONE', #8935 ) ;
#3572 = FACE_BOUND ( 'NONE', #2762, .T. ) ;
#3573 = AXIS2_PLACEMENT_3D ( 'NONE', #2398, #9006, #669 ) ;
#3574 = SURFACE_STYLE_FILL_AREA ( #2362 ) ;
#3575 = ORIENTED_EDGE ( 'NONE', *, *, #3988, .T. ) ;
#3576 = CARTESIAN_POINT ( 'NONE',  ( -1027.375436305353333, 71.63039521860234515, -152.5758913445296230 ) ) ;
#3577 = CARTESIAN_POINT ( 'NONE',  ( -20.75789059648688095, 180.8764387032748004, -123.4649828651695458 ) ) ;
#3578 = ORIENTED_EDGE ( 'NONE', *, *, #2552, .T. ) ;
#3579 = CIRCLE ( 'NONE', #4600, 30.00000000000021316 ) ;
#3580 = ORIENTED_EDGE ( 'NONE', *, *, #7508, .T. ) ;
#3581 = VECTOR ( 'NONE', #11319, 1000.000000000000000 ) ;
#3582 = CARTESIAN_POINT ( 'NONE',  ( -21.06729583384051097, 179.4139655881280078, -126.1965993184190040 ) ) ;
#3583 = CARTESIAN_POINT ( 'NONE',  ( -27.10787553788293280, 180.2041921146317236, -137.3302880892917983 ) ) ;
#3584 = EDGE_CURVE ( 'NONE', #4959, #8782, #4127, .T. ) ;
#3585 = VERTEX_POINT ( 'NONE', #11797 ) ;
#3586 = EDGE_CURVE ( 'NONE', #864, #9127, #3687, .T. ) ;
#3587 = CARTESIAN_POINT ( 'NONE',  ( -372.4126920328553183, 63.14209089232701899, -145.5554648177819388 ) ) ;
#3588 = LINE ( 'NONE', #2674, #1839 ) ;
#3589 =( REPRESENTATION_RELATIONSHIP ('NONE','NONE', #12149, #2032 ) REPRESENTATION_RELATIONSHIP_WITH_TRANSFORMATION ( #1156 )SHAPE_REPRESENTATION_RELATIONSHIP( ) );
#3590 = DIRECTION ( 'NONE',  ( -8.163404592832030268E-17, 1.000000000000000000, -0.000000000000000000 ) ) ;
#3591 = VERTEX_POINT ( 'NONE', #9998 ) ;
#3592 = CIRCLE ( 'NONE', #43, 7.500000000000007105 ) ;
#3593 = EDGE_CURVE ( 'NONE', #586, #864, #1530, .T. ) ;
#3594 = CARTESIAN_POINT ( 'NONE',  ( 9.184850993605161750E-16, 11.99999999999999645, -133.9213562373095101 ) ) ;
#3595 = CARTESIAN_POINT ( 'NONE',  ( 0.5612050131687977839, 4.355613924421556149, 8.999999999999998224 ) ) ;
#3596 = FACE_OUTER_BOUND ( 'NONE', #10705, .T. ) ;
#3597 = CARTESIAN_POINT ( 'NONE',  ( 6.247927005943220505E-13, 164.0000000000000000, -66.42135623730948168 ) ) ;
#3598 = CARTESIAN_POINT ( 'NONE',  ( -1062.301584968951602, 67.66927912025059300, -96.78565065507969223 ) ) ;
#3599 = DIRECTION ( 'NONE',  ( 0.000000000000000000, 1.000000000000000000, 0.000000000000000000 ) ) ;
#3600 = DIRECTION ( 'NONE',  ( 0.000000000000000000, 0.000000000000000000, 1.000000000000000000 ) ) ;
#3601 = SHAPE_REPRESENTATION ( 'Cast Iron Base Mounting Frame', ( #11957 ), #2892 ) ;
#3602 = EDGE_CURVE ( 'NONE', #3290, #6830, #7963, .T. ) ;
#3603 = EDGE_LOOP ( 'NONE', ( #4056, #3046, #10613 ) ) ;
#3604 = CARTESIAN_POINT ( 'NONE',  ( -370.1937529848235044, 107.5001225471108626, -132.1631802120997747 ) ) ;
#3605 = ORIENTED_EDGE ( 'NONE', *, *, #12191, .T. ) ;
#3606 = CARTESIAN_POINT ( 'NONE',  ( 0.000000000000000000, 12.00000000000000000, -89.68077099980401101 ) ) ;
#3607 = CARTESIAN_POINT ( 'NONE',  ( -997.0443963278638648, 49.75991663364290929, -103.3307627799637487 ) ) ;
#3608 = VECTOR ( 'NONE', #11555, 1000.000000000000000 ) ;
#3609 = CARTESIAN_POINT ( 'NONE',  ( -6.106226635438360972E-13, 12.00000000000000000, -252.1807709998039115 ) ) ;
#3610 = DIRECTION ( 'NONE',  ( -8.163404592832031500E-17, 1.000000000000000000, 0.000000000000000000 ) ) ;
#3611 = CARTESIAN_POINT ( 'NONE',  ( -126.4213562373094959, 0.000000000000000000, 2.255140518769849223E-14 ) ) ;
#3612 = CARTESIAN_POINT ( 'NONE',  ( -825.1499223856426397, 73.84923531294184329, -106.4169293550701951 ) ) ;
#3613 = CARTESIAN_POINT ( 'NONE',  ( -19.93794579528156419, 178.4740307436693740, -123.1021291661558195 ) ) ;
#3614 = CARTESIAN_POINT ( 'NONE',  ( -825.4626643026864485, 73.93730723265402105, -142.9841191000401750 ) ) ;
#3615 = VECTOR ( 'NONE', #6875, 1000.000000000000000 ) ;
#3616 = ORIENTED_EDGE ( 'NONE', *, *, #11937, .F. ) ;
#3617 = VERTEX_POINT ( 'NONE', #8789 ) ;
#3618 = DIRECTION ( 'NONE',  ( -0.000000000000000000, -0.000000000000000000, -1.000000000000000000 ) ) ;
#3619 = CARTESIAN_POINT ( 'NONE',  ( 4.808665244885994618E-14, -494.9999999999998863, 141.4213562373094817 ) ) ;
#3620 = AXIS2_PLACEMENT_3D ( 'NONE', #3023, #1981, #3140 ) ;
#3621 = ORIENTED_EDGE ( 'NONE', *, *, #1457, .F. ) ;
#3622 = CARTESIAN_POINT ( 'NONE',  ( -247.5000000000000000, 24.00000000000000711, -126.4213562373078190 ) ) ;
#3623 = CARTESIAN_POINT ( 'NONE',  ( -1013.875822516560447, 120.2710389253235519, -124.6807709998039257 ) ) ;
#3624 = CARTESIAN_POINT ( 'NONE',  ( 21.06618838917721348, 180.8542587794627821, -126.2858731283988618 ) ) ;
#3625 = CARTESIAN_POINT ( 'NONE',  ( 57.50000000000000000, 0.000000000000000000, 0.000000000000000000 ) ) ;
#3626 = CARTESIAN_POINT ( 'NONE',  ( -154.5043356068770493, 0.000000000000000000, -109.5666613060160586 ) ) ;
#3627 = AXIS2_PLACEMENT_3D ( 'NONE', #4275, #550, #8101 ) ;
#3628 = AXIS2_PLACEMENT_3D ( 'NONE', #2437, #519, #5337 ) ;
#3629 = VECTOR ( 'NONE', #7890, 1000.000000000000000 ) ;
#3630 = CARTESIAN_POINT ( 'NONE',  ( 20.91924760697977703, 181.5974164329501264, -124.2866227082428736 ) ) ;
#3631 = ORIENTED_EDGE ( 'NONE', *, *, #1407, .F. ) ;
#3632 = VERTEX_POINT ( 'NONE', #1368 ) ;
#3633 = CARTESIAN_POINT ( 'NONE',  ( -1030.931480980267906, 117.9615145441170654, -124.6807709998043521 ) ) ;
#3634 = DIRECTION ( 'NONE',  ( 0.000000000000000000, 0.000000000000000000, 1.000000000000000000 ) ) ;
#3635 = DIRECTION ( 'NONE',  ( 0.000000000000000000, 0.000000000000000000, -1.000000000000000000 ) ) ;
#3636 = CARTESIAN_POINT ( 'NONE',  ( -1065.000000000007731, 93.55451860843886891, -152.5758913445290830 ) ) ;
#3637 = AXIS2_PLACEMENT_3D ( 'NONE', #4591, #1065, #4940 ) ;
#3638 = PRESENTATION_STYLE_ASSIGNMENT (( #8363 ) ) ;
#3639 = DIRECTION ( 'NONE',  ( -0.000000000000000000, -1.000000000000000000, -0.000000000000000000 ) ) ;
#3640 = AXIS2_PLACEMENT_3D ( 'NONE', #736, #9264, #806 ) ;
#3641 = CARTESIAN_POINT ( 'NONE',  ( -903.2629211055218548, 97.63080833215174437, -154.2940595301276971 ) ) ;
#3642 = FACE_OUTER_BOUND ( 'NONE', #1663, .T. ) ;
#3643 = EDGE_LOOP ( 'NONE', ( #11417, #7051, #4704, #5616 ) ) ;
#3644 = CARTESIAN_POINT ( 'NONE',  ( -819.0860990673882043, 77.05720446847304572, -94.68731928646728591 ) ) ;
#3645 = ADVANCED_FACE ( 'NONE', ( #9772 ), #4534, .T. ) ;
#3646 = CARTESIAN_POINT ( 'NONE',  ( -372.8197369114613480, 99.38977441760248155, -147.2377432227614520 ) ) ;
#3647 = EDGE_LOOP ( 'NONE', ( #5089, #5481, #1564, #9524, #10935 ) ) ;
#3648 = CARTESIAN_POINT ( 'NONE',  ( -1065.000000000008868, 82.00000000000028422, -154.8742214401231081 ) ) ;
#3649 = EDGE_CURVE ( 'NONE', #9395, #495, #2950, .T. ) ;
#3650 = CARTESIAN_POINT ( 'NONE',  ( 19.86004308345772529, 179.1220966913736277, -127.0453612081607844 ) ) ;
#3651 = VERTEX_POINT ( 'NONE', #2181 ) ;
#3652 = CIRCLE ( 'NONE', #5223, 7.500000000000020428 ) ;
#3653 = AXIS2_PLACEMENT_3D ( 'NONE', #7081, #11899, #2383 ) ;
#3654 = EDGE_LOOP ( 'NONE', ( #4821, #4784, #3184, #7823 ) ) ;
#3655 = EDGE_CURVE ( 'NONE', #9404, #2620, #1429, .T. ) ;
#3656 = CARTESIAN_POINT ( 'NONE',  ( -827.1569714199418968, 74.92915896789017438, -105.9707980921570112 ) ) ;
#3657 = CARTESIAN_POINT ( 'NONE',  ( -928.3598895238005753, 61.90886769853032945, -136.2353035311983263 ) ) ;
#3658 = ORIENTED_EDGE ( 'NONE', *, *, #6321, .F. ) ;
#3659 = CARTESIAN_POINT ( 'NONE',  ( -382.1381191270742761, 67.86032419806703331, -138.8291321671420633 ) ) ;
#3660 = DIRECTION ( 'NONE',  ( -1.186840563529527301E-16, 1.000000000000000000, -0.000000000000000000 ) ) ;
#3661 = CARTESIAN_POINT ( 'NONE',  ( 154.5043356068769071, 0.000000000000000000, -102.0666613060171386 ) ) ;
#3662 =( GEOMETRIC_REPRESENTATION_CONTEXT ( 3 ) GLOBAL_UNCERTAINTY_ASSIGNED_CONTEXT ( ( #3234 ) ) GLOBAL_UNIT_ASSIGNED_CONTEXT ( ( #2382, #6221, #588 ) ) REPRESENTATION_CONTEXT ( 'NONE', 'WORKASPACE' ) );
#3663 = CARTESIAN_POINT ( 'NONE',  ( 0.000000000000000000, 12.00000000000000000, -264.6807709998040536 ) ) ;
#3664 = B_SPLINE_CURVE_WITH_KNOTS ( 'NONE', 3,
 ( #2011, #8744, #1953, #5025, #324, #2191, #11526, #4110, #4793, #11403, #2998, #5833, #8563, #2881, #6703, #84, #2075, #8691, #4846, #8627, #5713, #200, #3055, #5897, #10595, #141, #2135, #6827, #9671, #1209, #5769, #3924, #10655, #7695, #11466, #11593, #3110, #6885, #8859, #1562, #5325, #4165, #3397, #8975, #3225, #2486, #2371, #2421, #7188, #11884, #501, #6201 ),
 .UNSPECIFIED., .F., .F.,
 ( 4, 2, 2, 2, 2, 2, 2, 2, 2, 2, 2, 2, 2, 2, 2, 2, 2, 2, 2, 2, 2, 2, 2, 2, 2, 4 ),
 ( 0.07032306561503316733, 0.07210969465899567943, 0.07389632370295820540, 0.07568295274692071750, 0.07746958179088322960, 0.08104283987880832318, 0.08461609796673341677, 0.08640272701069594274, 0.08818935605465848260, 0.09176261414258357618, 0.09354924318654614379, 0.09444255770852742760, 0.09533587223050871140, 0.09890913031843383274, 0.1006957593623963865, 0.1024823884063589263, 0.1060556464942840477, 0.1078422755382466014, 0.1096289045822091412, 0.1132021626701343042, 0.1149887917140968996, 0.1167754207580594672, 0.1203486788459845747, 0.1221353078899471561, 0.1239219369339097376, 0.1274951950218348451 ),
 .UNSPECIFIED. ) ;
#3665 = DIRECTION ( 'NONE',  ( 0.7071067811865472397, 0.000000000000000000, -0.7071067811865479058 ) ) ;
#3666 = EDGE_CURVE ( 'NONE', #2997, #90, #8481, .T. ) ;
#3667 = ADVANCED_FACE ( 'NONE', ( #1252 ), #2359, .F. ) ;
#3668 = CARTESIAN_POINT ( 'NONE',  ( 0.8038475772933606489, 5.196152422706624918, 8.999999999999998224 ) ) ;
#3669 = CARTESIAN_POINT ( 'NONE',  ( 19.98760292801598126, 179.0152138695270594, -125.5961219049576982 ) ) ;
#3670 = PRODUCT_DEFINITION_FORMATION_WITH_SPECIFIED_SOURCE ( 'ANY', '', #118, .NOT_KNOWN. ) ;
#3671 = CARTESIAN_POINT ( 'NONE',  ( -1025.595947590972401, 58.17469240935120922, -107.9061927053327707 ) ) ;
#3672 = CARTESIAN_POINT ( 'NONE',  ( 1.734723475976807094E-15, 180.2041921146324910, -179.7948474705909234 ) ) ;
#3673 = CARTESIAN_POINT ( 'NONE',  ( -379.1619848709566440, 102.0000000000000142, -124.6807709998038405 ) ) ;
#3674 = PRODUCT_DEFINITION ( 'UNKNOWN', '', #509, #6655 ) ;
#3675 = AXIS2_PLACEMENT_3D ( 'NONE', #10883, #7934, #3221 ) ;
#3676 = ORIENTED_EDGE ( 'NONE', *, *, #9653, .T. ) ;
#3677 = CARTESIAN_POINT ( 'NONE',  ( -828.0828412852908968, 81.30646073758796888, -144.6692115456658598 ) ) ;
#3678 = CARTESIAN_POINT ( 'NONE',  ( 0.000000000000000000, -485.4999999999998863, 126.4213562373094959 ) ) ;
#3679 = VERTEX_POINT ( 'NONE', #4096 ) ;
#3680 = CARTESIAN_POINT ( 'NONE',  ( -956.7203770923135835, 58.97922774997691420, -103.3307627799636919 ) ) ;
#3681 = CARTESIAN_POINT ( 'NONE',  ( 0.000000000000000000, 81.99999999999995737, -159.6807709998038547 ) ) ;
#3682 = LINE ( 'NONE', #9439, #10211 ) ;
#3683 = CARTESIAN_POINT ( 'NONE',  ( 20.71964524312746647, 180.2041921146487766, -123.3053720114591414 ) ) ;
#3684 = AXIS2_PLACEMENT_3D ( 'NONE', #7324, #11026, #11155 ) ;
#3685 = EDGE_CURVE ( 'NONE', #5830, #9411, #11636, .T. ) ;
#3686 = DIRECTION ( 'NONE',  ( -0.7071067811865473507, 0.000000000000000000, 0.7071067811865477948 ) ) ;
#3687 = B_SPLINE_CURVE_WITH_KNOTS ( 'NONE', 3,
 ( #4316, #3313, #11856, #9934, #10858, #6233, #9815, #7911 ),
 .UNSPECIFIED., .F., .F.,
 ( 4, 2, 2, 4 ),
 ( 0.06374494753957145321, 0.06538947705843686786, 0.06703400657730228251, 0.07032306561503316733 ),
 .UNSPECIFIED. ) ;
#3688 = CARTESIAN_POINT ( 'NONE',  ( -818.9891295040788464, 77.37577012655981434, -105.2199448511378819 ) ) ;
#3689 = CARTESIAN_POINT ( 'NONE',  ( -20.76475501013377212, 179.4826916305587474, -123.4955357876650197 ) ) ;
#3690 = CARTESIAN_POINT ( 'NONE',  ( -824.6569351206097735, 73.74060470499414066, -142.8957018107298040 ) ) ;
#3691 = EDGE_LOOP ( 'NONE', ( #9564, #6137, #10492, #8006 ) ) ;
#3692 = CARTESIAN_POINT ( 'NONE',  ( -373.6433083154181531, 68.25182830884359930, -150.2667927013042970 ) ) ;
#3693 = CARTESIAN_POINT ( 'NONE',  ( -371.5221853768310325, 103.7913954946613728, -107.9473401059475890 ) ) ;
#3694 = CIRCLE ( 'NONE', #9224, 7.500000000000007105 ) ;
#3695 = ORIENTED_EDGE ( 'NONE', *, *, #2552, .F. ) ;
#3696 = CARTESIAN_POINT ( 'NONE',  ( -852.9318753287178652, 113.3383058689773151, -107.9061927053323302 ) ) ;
#3697 = DIRECTION ( 'NONE',  ( 0.000000000000000000, 0.000000000000000000, 1.000000000000000000 ) ) ;
#3698 = CARTESIAN_POINT ( 'NONE',  ( 20.79565762252865468, 181.1410762094974700, -123.6324090417393649 ) ) ;
#3699 = AXIS2_PLACEMENT_3D ( 'NONE', #6916, #9004, #2284 ) ;
#3700 = ORIENTED_EDGE ( 'NONE', *, *, #10907, .F. ) ;
#3701 = VECTOR ( 'NONE', #3851, 999.9999999999998863 ) ;
#3702 = ORIENTED_EDGE ( 'NONE', *, *, #7352, .F. ) ;
#3703 = CARTESIAN_POINT ( 'NONE',  ( 1.387778780781445676E-14, -58.00000000000000711, 126.4213562373094959 ) ) ;
#3704 = DIRECTION ( 'NONE',  ( -8.163404592832030268E-17, 1.000000000000000000, -0.000000000000000000 ) ) ;
#3705 = CARTESIAN_POINT ( 'NONE',  ( -795.0000000000094360, 82.00000000000081002, -154.8742214401225397 ) ) ;
#3706 = CARTESIAN_POINT ( 'NONE',  ( -372.4693655937733183, 101.8286029160101549, -121.6495295015975273 ) ) ;
#3707 = DIRECTION ( 'NONE',  ( 0.000000000000000000, -1.189524669241239115E-16, 1.000000000000000000 ) ) ;
#3708 = CARTESIAN_POINT ( 'NONE',  ( -1025.928429817215147, 97.79385104913471594, -152.5758913445291398 ) ) ;
#3709 = CARTESIAN_POINT ( 'NONE',  ( -126.4213562373094959, -6.000000000000000000, 7.500000000000035527 ) ) ;
#3710 = ORIENTED_EDGE ( 'NONE', *, *, #9999, .F. ) ;
#3711 = DIRECTION ( 'NONE',  ( -0.000000000000000000, 1.000000000000000000, 7.930164461608263644E-17 ) ) ;
#3712 = CIRCLE ( 'NONE', #12000, 9.000000000000000000 ) ;
#3713 = CARTESIAN_POINT ( 'NONE',  ( -383.7289910790237855, 91.48765077515149358, -142.2992162448462068 ) ) ;
#3714 = ORIENTED_EDGE ( 'NONE', *, *, #10976, .F. ) ;
#3715 = CARTESIAN_POINT ( 'NONE',  ( -1031.956718292102323, 74.21439239895576634, -154.2940595301282656 ) ) ;
#3716 = VERTEX_POINT ( 'NONE', #7926 ) ;
#3717 = CIRCLE ( 'NONE', #6283, 30.00000000000021316 ) ;
#3718 = ORIENTED_EDGE ( 'NONE', *, *, #5149, .T. ) ;
#3719 = VECTOR ( 'NONE', #6238, 1000.000000000000000 ) ;
#3720 = EDGE_CURVE ( 'NONE', #2170, #5214, #3923, .T. ) ;
#3721 = CARTESIAN_POINT ( 'NONE',  ( -827.1410867119041086, 82.43389265416672629, -144.6774099844745365 ) ) ;
#3722 = CARTESIAN_POINT ( 'NONE',  ( -19.96948860049111474, 182.3247467770471530, -123.5689856398053763 ) ) ;
#3723 = CARTESIAN_POINT ( 'NONE',  ( 6.247927005943220505E-13, 0.000000000000000000, -66.42135623730949590 ) ) ;
#3724 = FACE_BOUND ( 'NONE', #2034, .T. ) ;
#3725 = CARTESIAN_POINT ( 'NONE',  ( -901.9718911164696920, 59.00785292138922244, -136.2353035311984115 ) ) ;
#3726 = EDGE_CURVE ( 'NONE', #154, #6278, #1172, .T. ) ;
#3727 = CARTESIAN_POINT ( 'NONE',  ( -372.4202255147081360, 61.99933121941937486, -123.1818127415012896 ) ) ;
#3728 = DIRECTION ( 'NONE',  ( -1.000000000000000000, -0.000000000000000000, -0.000000000000000000 ) ) ;
#3729 = CYLINDRICAL_SURFACE ( 'NONE', #11609, 7.500000000000007105 ) ;
#3730 = AXIS2_PLACEMENT_3D ( 'NONE', #7218, #1297, #10923 ) ;
#3731 = CIRCLE ( 'NONE', #12217, 175.0000000000000000 ) ;
#3732 = DIRECTION ( 'NONE',  ( -1.000000000000000000, 0.000000000000000000, 0.000000000000000000 ) ) ;
#3733 = CARTESIAN_POINT ( 'NONE',  ( 0.3593302862868652525, 3.504574740656557275, 9.000000000000001776 ) ) ;
#3734 = DIRECTION ( 'NONE',  ( -0.000000000000000000, -1.000000000000000000, -0.000000000000000000 ) ) ;
#3735 = CARTESIAN_POINT ( 'NONE',  ( -1062.810894920125520, 52.92335929224832825, -107.9061927053327139 ) ) ;
#3736 = CARTESIAN_POINT ( 'NONE',  ( 0.07661102881317168045, -6.914460432017388136, -6.023803224821241642 ) ) ;
#3737 = CARTESIAN_POINT ( 'NONE',  ( -305.0000000000000568, 81.99999999999995737, -89.68077099980384048 ) ) ;
#3738 = CARTESIAN_POINT ( 'NONE',  ( -817.1493800258450619, 27.50875274330017461, -126.6442663926291630 ) ) ;
#3739 = CARTESIAN_POINT ( 'NONE',  ( -821.6112282492948680, 83.16771792585157641, -144.6470480974983843 ) ) ;
#3740 = ORIENTED_EDGE ( 'NONE', *, *, #6969, .T. ) ;
#3741 = FACE_BOUND ( 'NONE', #798, .T. ) ;
#3742 = EDGE_CURVE ( 'NONE', #2820, #1615, #9430, .T. ) ;
#3743 = DIRECTION ( 'NONE',  ( 0.9994711065474021217, -8.212794959806906007E-17, -0.03251933543158291168 ) ) ;
#3744 = VERTEX_POINT ( 'NONE', #554 ) ;
#3745 = CARTESIAN_POINT ( 'NONE',  ( -823.8285638327247398, 78.67432280806536937, -158.6807709998041673 ) ) ;
#3746 = CARTESIAN_POINT ( 'NONE',  ( -1047.844889418690855, 56.55730854968127375, -99.57582448894520155 ) ) ;
#3747 = AXIS2_PLACEMENT_3D ( 'NONE', #5667, #11353, #1967 ) ;
#3748 = CARTESIAN_POINT ( 'NONE',  ( -818.8285638327206470, 78.67432280806529832, -264.6807709998040536 ) ) ;
#3749 = CARTESIAN_POINT ( 'NONE',  ( -154.5043356068770493, 12.00000000000000000, -102.0666613060160302 ) ) ;
#3750 = CARTESIAN_POINT ( 'NONE',  ( -826.9035580923963380, 74.71835857218523813, -106.0523996049646769 ) ) ;
#3751 = DIRECTION ( 'NONE',  ( 2.081668171172161734E-17, 4.930380657631307143E-31, -1.000000000000000000 ) ) ;
#3752 = ORIENTED_EDGE ( 'NONE', *, *, #9016, .T. ) ;
#3753 = CARTESIAN_POINT ( 'NONE',  ( -2.775557561562891351E-14, 139.9999999999999716, -159.6807709998038547 ) ) ;
#3754 = ADVANCED_FACE ( 'NONE', ( #4334 ), #2591, .F. ) ;
#3755 = EDGE_CURVE ( 'NONE', #10145, #4307, #10832, .T. ) ;
#3756 = EDGE_LOOP ( 'NONE', ( #7145, #8148, #2298, #9289 ) ) ;
#3757 = CARTESIAN_POINT ( 'NONE',  ( -1025.044148074454370, 113.2108726315405960, -107.9061927053325007 ) ) ;
#3758 = MANIFOLD_SOLID_BREP ( 'Boss-Extrude7', #9857 ) ;
#3759 = CARTESIAN_POINT ( 'NONE',  ( -97.50000000000000000, 152.0000000000000000, -126.4213562373088564 ) ) ;
#3760 = LINE ( 'NONE', #8477, #10027 ) ;
#3761 = CARTESIAN_POINT ( 'NONE',  ( 21.04760817881890844, 181.6185052388174199, -125.4224630414783945 ) ) ;
#3762 = CARTESIAN_POINT ( 'NONE',  ( -1010.922847972425529, 120.6260792194948550, -124.6807709998039542 ) ) ;
#3763 = ORIENTED_EDGE ( 'NONE', *, *, #3155, .T. ) ;
#3764 = CARTESIAN_POINT ( 'NONE',  ( -120.8820948793972434, 0.000000000000000000, -186.6989091883324363 ) ) ;
#3765 =( REPRESENTATION_RELATIONSHIP ('NONE','NONE', #12149, #3601 ) REPRESENTATION_RELATIONSHIP_WITH_TRANSFORMATION ( #10659 )SHAPE_REPRESENTATION_RELATIONSHIP( ) );
#3766 = CYLINDRICAL_SURFACE ( 'NONE', #1968, 7.500000000000007105 ) ;
#3767 = CARTESIAN_POINT ( 'NONE',  ( 21.06714545844871367, 179.4370239411119030, -126.2109676220344596 ) ) ;
#3768 = CARTESIAN_POINT ( 'NONE',  ( -927.4753839990684128, 92.66010094724849466, -154.8742214401223691 ) ) ;
#3769 =( NAMED_UNIT ( * ) SI_UNIT ( $, .STERADIAN. ) SOLID_ANGLE_UNIT ( ) );
#3770 = CARTESIAN_POINT ( 'NONE',  ( -144.0488662551579182, 0.000000000000000000, -154.4077238332691877 ) ) ;
#3771 = CARTESIAN_POINT ( 'NONE',  ( 9.184850993605161750E-16, 152.0000000000000284, -133.9213562373095101 ) ) ;
#3772 = ORIENTED_EDGE ( 'NONE', *, *, #253, .T. ) ;
#3773 = CARTESIAN_POINT ( 'NONE',  ( -380.8316613798133403, 98.99442196914210967, -135.2453119940010140 ) ) ;
#3774 = ORIENTED_EDGE ( 'NONE', *, *, #8809, .F. ) ;
#3775 = CARTESIAN_POINT ( 'NONE',  ( -1012.828629370413182, 79.69572830938452057, -154.2940595301284361 ) ) ;
#3776 = LINE ( 'NONE', #5003, #1618 ) ;
#3777 = ORIENTED_EDGE ( 'NONE', *, *, #7850, .F. ) ;
#3778 = ORIENTED_EDGE ( 'NONE', *, *, #2102, .T. ) ;
#3779 = CARTESIAN_POINT ( 'NONE',  ( -825.6238610960883761, 74.00482032089516338, -106.3482309385110511 ) ) ;
#3780 = AXIS2_PLACEMENT_3D ( 'NONE', #5345, #1522, #8085 ) ;
#3781 = EDGE_LOOP ( 'NONE', ( #3990, #2108, #4113, #8285 ) ) ;
#3782 = CARTESIAN_POINT ( 'NONE',  ( -375.0054150261470340, 82.02639447815485596, -154.6972847430876925 ) ) ;
#3783 = CARTESIAN_POINT ( 'NONE',  ( 7.500000000000000000, 0.000000000000000000, 0.000000000000000000 ) ) ;
#3784 = CARTESIAN_POINT ( 'NONE',  ( -374.8879932666449122, 77.11444321722318307, -105.2520959535442557 ) ) ;
#3785 = CARTESIAN_POINT ( 'NONE',  ( -1065.000000000006366, 82.00000000000036948, -124.6807709998044231 ) ) ;
#3786 = DIRECTION ( 'NONE',  ( -0.000000000000000000, -1.000000000000000000, -0.000000000000000000 ) ) ;
#3787 = VERTEX_POINT ( 'NONE', #7173 ) ;
#3788 = EDGE_CURVE ( 'NONE', #6435, #8054, #7808, .T. ) ;
#3789 = AXIS2_PLACEMENT_3D ( 'NONE', #11053, #11859, #5489 ) ;
#3790 = DIRECTION ( 'NONE',  ( 0.000000000000000000, -1.156482317317870246E-16, 1.000000000000000000 ) ) ;
#3791 = CARTESIAN_POINT ( 'NONE',  ( 21.06714545844871722, 179.4370239411119030, -126.2109676220344596 ) ) ;
#3792 = CARTESIAN_POINT ( 'NONE',  ( -953.8433812051914629, 65.95343150956773570, -99.57582448894520155 ) ) ;
#3793 = CARTESIAN_POINT ( 'NONE',  ( -827.1368241426298482, 82.43785830827036420, -104.6842000310834777 ) ) ;
#3794 = CARTESIAN_POINT ( 'NONE',  ( -7.499999999999994671, -9.213203435596451385, -126.4213562373094959 ) ) ;
#3795 = CARTESIAN_POINT ( 'NONE',  ( -1057.832023714520119, 42.29985473022490794, -126.6442663926294330 ) ) ;
#3796 = AXIS2_PLACEMENT_3D ( 'NONE', #8383, #5519, #834 ) ;
#3797 = ORIENTED_EDGE ( 'NONE', *, *, #2991, .F. ) ;
#3798 = CARTESIAN_POINT ( 'NONE',  ( -819.8521517457879781, 81.72352651608152030, -144.6807563939346437 ) ) ;
#3799 = DIRECTION ( 'NONE',  ( 0.000000000000000000, 0.000000000000000000, 1.000000000000000000 ) ) ;
#3800 = SURFACE_SIDE_STYLE ('',( #11407 ) ) ;
#3801 = ORIENTED_EDGE ( 'NONE', *, *, #4816, .T. ) ;
#3802 = CARTESIAN_POINT ( 'NONE',  ( -954.2862664537825594, 55.36536439393501041, -107.9061927053324439 ) ) ;
#3803 = EDGE_CURVE ( 'NONE', #5876, #1690, #5511, .T. ) ;
#3804 = CARTESIAN_POINT ( 'NONE',  ( 35.00000000000000000, 163.9999999999999716, 190.3192290001959748 ) ) ;
#3805 = CYLINDRICAL_SURFACE ( 'NONE', #7967, 35.00000000000002842 ) ;
#3806 = DIRECTION ( 'NONE',  ( 0.000000000000000000, 1.000000000000000000, 0.000000000000000000 ) ) ;
#3807 = ADVANCED_FACE ( 'NONE', ( #10268 ), #10840, .T. ) ;
#3808 = PRODUCT_DEFINITION_CONTEXT ( 'detailed design', #9041, 'design' ) ;
#3809 = DIRECTION ( 'NONE',  ( 1.000000000000000000, 0.000000000000000000, 0.000000000000000000 ) ) ;
#3810 = CARTESIAN_POINT ( 'NONE',  ( -19.99208445718651106, 177.7326588799362810, -125.2637803837037325 ) ) ;
#3811 = DIRECTION ( 'NONE',  ( -8.163404592832030268E-17, 1.000000000000000000, -0.000000000000000000 ) ) ;
#3812 = VERTEX_POINT ( 'NONE', #1603 ) ;
#3813 = CARTESIAN_POINT ( 'NONE',  ( -374.8738968220091010, 87.13760577545254193, -105.3208045665617050 ) ) ;
#3814 = TOROIDAL_SURFACE ( 'NONE', #10723, 14.02076803445813269, 1.499999999999998002 ) ;
#3815 = ORIENTED_EDGE ( 'NONE', *, *, #7386, .T. ) ;
#3816 = CARTESIAN_POINT ( 'NONE',  ( -926.6866529578969676, 120.3119365386820192, -107.9061927053322734 ) ) ;
#3817 = CARTESIAN_POINT ( 'NONE',  ( 35.00000000000000000, 12.00000000000000000, 40.70327710424895429 ) ) ;
#3818 = CARTESIAN_POINT ( 'NONE',  ( -1030.944970944897250, 117.4714819019839354, -130.5712005305406649 ) ) ;
#3819 = CARTESIAN_POINT ( 'NONE',  ( 19.90005091283025962, 178.5478491056598500, -126.6842376513516513 ) ) ;
#3820 = EDGE_CURVE ( 'NONE', #9670, #5146, #7293, .T. ) ;
#3821 = CIRCLE ( 'NONE', #4218, 7.500000000000007105 ) ;
#3822 = EDGE_CURVE ( 'NONE', #12001, #7478, #1372, .T. ) ;
#3823 = CARTESIAN_POINT ( 'NONE',  ( -1054.380968608931425, 114.0683136310379524, -124.6807709998043663 ) ) ;
#3824 = EDGE_LOOP ( 'NONE', ( #1784, #9547, #6141, #9948, #712, #7860 ) ) ;
#3825 = CARTESIAN_POINT ( 'NONE',  ( -365.0000000000000568, 81.99999999999997158, -124.6807709998038405 ) ) ;
#3826 = FACE_BOUND ( 'NONE', #7708, .T. ) ;
#3827 = CARTESIAN_POINT ( 'NONE',  ( -1061.104375862961888, 103.3839434440459968, -146.0307792196447565 ) ) ;
#3828 = EDGE_CURVE ( 'NONE', #4476, #7628, #4136, .T. ) ;
#3829 = CARTESIAN_POINT ( 'NONE',  ( 11.89695805161205655, 180.2041921146325762, -183.6976696918629557 ) ) ;
#3830 = ADVANCED_BREP_SHAPE_REPRESENTATION ( '', ( #3758, #8147, #11957 ), #2892 ) ;
#3831 = DIRECTION ( 'NONE',  ( -1.186840563529527301E-16, 1.000000000000000000, -0.000000000000000000 ) ) ;
#3832 = DIRECTION ( 'NONE',  ( 1.000000000000000000, 0.000000000000000000, -0.000000000000000000 ) ) ;
#3833 = ORIENTED_EDGE ( 'NONE', *, *, #5265, .T. ) ;
#3834 = CIRCLE ( 'NONE', #7584, 7.500000000000007105 ) ;
#3835 = CIRCLE ( 'NONE', #1086, 81.99999999999998579 ) ;
#3836 = CARTESIAN_POINT ( 'NONE',  ( -372.9336440560613255, 100.1246349412789556, -133.3251676657040150 ) ) ;
#3837 = FACE_OUTER_BOUND ( 'NONE', #8759, .T. ) ;
#3838 = EDGE_LOOP ( 'NONE', ( #9982, #11366, #11265, #4376 ) ) ;
#3839 = EDGE_CURVE ( 'NONE', #1374, #9727, #4573, .T. ) ;
#3840 = EDGE_LOOP ( 'NONE', ( #10910, #3537 ) ) ;
#3841 = CARTESIAN_POINT ( 'NONE',  ( 20.80735028308761869, 179.2184937932714490, -123.6883961446522022 ) ) ;
#3842 = AXIS2_PLACEMENT_3D ( 'NONE', #7204, #9111, #2499 ) ;
#3843 = CARTESIAN_POINT ( 'NONE',  ( -19.99390413358784357, 181.6003807074973793, -125.2540357159168423 ) ) ;
#3844 = AXIS2_PLACEMENT_3D ( 'NONE', #6142, #640, #7258 ) ;
#3845 = DIRECTION ( 'NONE',  ( -1.000000000000000000, 0.000000000000000000, 0.000000000000000000 ) ) ;
#3846 = CARTESIAN_POINT ( 'NONE',  ( -902.2382941300837729, 66.55116351576596401, -146.0307792196448986 ) ) ;
#3847 = ORIENTED_EDGE ( 'NONE', *, *, #2427, .T. ) ;
#3848 = CARTESIAN_POINT ( 'NONE',  ( -374.7692102046581795, 75.20231895184195992, -143.5370633296073493 ) ) ;
#3849 = PLANE ( 'NONE',  #11735 ) ;
#3850 = CARTESIAN_POINT ( 'NONE',  ( -374.4847994008925980, 73.48375005241382496, -96.28629692668562257 ) ) ;
#3851 = DIRECTION ( 'NONE',  ( 0.7071067811865479058, 0.000000000000000000, 0.7071067811865472397 ) ) ;
#3852 = ORIENTED_EDGE ( 'NONE', *, *, #3348, .T. ) ;
#3853 = AXIS2_PLACEMENT_3D ( 'NONE', #8253, #6326, #1823 ) ;
#3854 = CIRCLE ( 'NONE', #10167, 0.9999999999999991118 ) ;
#3855 = ORIENTED_EDGE ( 'NONE', *, *, #6665, .T. ) ;
#3856 = CARTESIAN_POINT ( 'NONE',  ( 19.99326885945900401, 178.8248732837839157, -125.2918954700392646 ) ) ;
#3857 = CARTESIAN_POINT ( 'NONE',  ( -1048.040919118596321, 50.77060569800394063, -103.3307627799636919 ) ) ;
#3858 = PLANE ( 'NONE',  #10505 ) ;
#3859 = CARTESIAN_POINT ( 'NONE',  ( -1021.637154595298057, 53.81063926482157456, -126.6442663926291630 ) ) ;
#3860 = MANIFOLD_SOLID_BREP ( 'Boss-Extrude1', #8083 ) ;
#3861 = ORIENTED_EDGE ( 'NONE', *, *, #391, .T. ) ;
#3862 = CARTESIAN_POINT ( 'NONE',  ( -826.3405481598731512, 83.00984762678820061, -144.6560901833814796 ) ) ;
#3863 = AXIS2_PLACEMENT_3D ( 'NONE', #2103, #10322, #8538 ) ;
#3864 = ORIENTED_EDGE ( 'NONE', *, *, #904, .T. ) ;
#3865 = SHAPE_DEFINITION_REPRESENTATION ( #10383, #6140 ) ;
#3866 = CARTESIAN_POINT ( 'NONE',  ( -370.0251988910513887, 107.9185164359716111, -129.9457498366273285 ) ) ;
#3867 = ORIENTED_EDGE ( 'NONE', *, *, #7290, .T. ) ;
#3868 = CARTESIAN_POINT ( 'NONE',  ( -975.7625022073081027, 55.15120678236761620, -99.57582448894500260 ) ) ;
#3869 = LINE ( 'NONE', #7761, #8276 ) ;
#3870 = CARTESIAN_POINT ( 'NONE',  ( -18.99999999999999645, 167.0000000000000000, -124.6807709998038405 ) ) ;
#3871 = DIRECTION ( 'NONE',  ( 0.000000000000000000, -1.156482317317870246E-16, 1.000000000000000000 ) ) ;
#3872 = CARTESIAN_POINT ( 'NONE',  ( -795.0000000000065938, 109.8950841424301217, -113.1262384684096105 ) ) ;
#3873 = DIRECTION ( 'NONE',  ( -1.000000000000000000, 0.000000000000000000, 0.000000000000000000 ) ) ;
#3874 = CARTESIAN_POINT ( 'NONE',  ( -19.95650872578057644, 177.9942513821760031, -126.0067755081681042 ) ) ;
#3875 = ADVANCED_FACE ( 'NONE', ( #9400 ), #8681, .T. ) ;
#3876 = EDGE_LOOP ( 'NONE', ( #3227, #1674 ) ) ;
#3877 = EDGE_CURVE ( 'NONE', #3054, #8695, #2751, .T. ) ;
#3878 = PRODUCT_DEFINITION_FORMATION_WITH_SPECIFIED_SOURCE ( 'ANY', '', #8619, .NOT_KNOWN. ) ;
#3879 = ORIENTED_EDGE ( 'NONE', *, *, #1026, .F. ) ;
#3880 = CARTESIAN_POINT ( 'NONE',  ( -1046.095701327177267, 109.2451008237761982, -107.9061927053324439 ) ) ;
#3881 = VECTOR ( 'NONE', #3786, 1000.000000000000000 ) ;
#3882 = CARTESIAN_POINT ( 'NONE',  ( 0.1469846612282494080, -8.891930899535433142, -2.598723904613006397 ) ) ;
#3883 = CARTESIAN_POINT ( 'NONE',  ( -974.2138504089066373, 120.9496320545085695, -136.2353035311977010 ) ) ;
#3884 = CARTESIAN_POINT ( 'NONE',  ( 20.00000000000000711, 177.6938224469233774, -124.9045029178196842 ) ) ;
#3885 = EDGE_CURVE ( 'NONE', #2975, #3899, #791, .T. ) ;
#3886 = CARTESIAN_POINT ( 'NONE',  ( -20.79945932778137063, 181.1616795883780071, -123.6498693937513025 ) ) ;
#3887 = EDGE_LOOP ( 'NONE', ( #9683, #1817 ) ) ;
#3888 = AXIS2_PLACEMENT_3D ( 'NONE', #9058, #3423, #8139 ) ;
#3889 = FACE_OUTER_BOUND ( 'NONE', #4143, .T. ) ;
#3890 = LINE ( 'NONE', #4991, #1759 ) ;
#3891 = CARTESIAN_POINT ( 'NONE',  ( -1065.000000000003411, 103.3499740386315580, -146.0307792196444154 ) ) ;
#3892 = DIRECTION ( 'NONE',  ( -1.000000000000000000, 0.000000000000000000, -6.195440985631454085E-17 ) ) ;
#3893 = ORIENTED_EDGE ( 'NONE', *, *, #5543, .T. ) ;
#3894 = ADVANCED_FACE ( 'NONE', ( #6554 ), #10320, .F. ) ;
#3895 = DIRECTION ( 'NONE',  ( -0.000000000000000000, -1.000000000000000000, -0.000000000000000000 ) ) ;
#3896 = CARTESIAN_POINT ( 'NONE',  ( -1031.086615573508880, 111.8776252365151009, -141.4553492942759760 ) ) ;
#3897 = CIRCLE ( 'NONE', #8453, 7.500000000000020428 ) ;
#3898 = FACE_BOUND ( 'NONE', #3938, .T. ) ;
#3899 = VERTEX_POINT ( 'NONE', #3829 ) ;
#3900 = EDGE_LOOP ( 'NONE', ( #10586, #2403, #5949, #10431 ) ) ;
#3901 = CARTESIAN_POINT ( 'NONE',  ( 19.96555171194421163, 178.1301448319365193, -123.4995670770394582 ) ) ;
#3902 = DIRECTION ( 'NONE',  ( 1.000000000000000000, 1.486905836551548832E-16, -0.000000000000000000 ) ) ;
#3903 = CARTESIAN_POINT ( 'NONE',  ( -19.97681936893992116, 182.4076374096303539, -123.7075806145273873 ) ) ;
#3904 = CARTESIAN_POINT ( 'NONE',  ( -380.8597684633047038, 98.93849339411727328, -135.3307194093575276 ) ) ;
#3905 = CARTESIAN_POINT ( 'NONE',  ( -928.1401715909056520, 69.16346707077036626, -146.0307792196452965 ) ) ;
#3906 = ORIENTED_EDGE ( 'NONE', *, *, #9393, .T. ) ;
#3907 = AXIS2_PLACEMENT_3D ( 'NONE', #4669, #6633, #836 ) ;
#3908 = CARTESIAN_POINT ( 'NONE',  ( -375.0012963295443456, 82.01691494583486985, -144.6876712114242594 ) ) ;
#3909 = DIRECTION ( 'NONE',  ( -0.000000000000000000, -1.000000000000000000, -0.000000000000000000 ) ) ;
#3910 = CARTESIAN_POINT ( 'NONE',  ( -373.7553986963736179, 68.76651228785951275, -98.69780169588010210 ) ) ;
#3912 = ADVANCED_FACE ( 'NONE', ( #1920 ), #4281, .T. ) ;
#3911 = CARTESIAN_POINT ( 'NONE',  ( 35.00000000000000000, 139.9999999999999716, -159.6807709998038547 ) ) ;
#3913 = ORIENTED_EDGE ( 'NONE', *, *, #11025, .T. ) ;
#3914 = CARTESIAN_POINT ( 'NONE',  ( -957.0819499390250940, 50.45265437475578807, -136.2353035311988663 ) ) ;
#3915 = AXIS2_PLACEMENT_3D ( 'NONE', #2250, #8118, #11883 ) ;
#3916 = CIRCLE ( 'NONE', #2520, 7.500000000000007105 ) ;
#3917 = ORIENTED_EDGE ( 'NONE', *, *, #9408, .T. ) ;
#3918 = EDGE_LOOP ( 'NONE', ( #5642, #3917 ) ) ;
#3919 = CARTESIAN_POINT ( 'NONE',  ( 9.381075359908434252E-13, -6.000000000000004441, -43.92135623730950300 ) ) ;
#3920 = CARTESIAN_POINT ( 'NONE',  ( -819.2376510598700179, 55.50059629688461627, -96.78565065507937959 ) ) ;
#3921 = CARTESIAN_POINT ( 'NONE',  ( -826.8820017809032379, 82.64709913614477443, -104.6904163631604092 ) ) ;
#3922 = ORIENTED_EDGE ( 'NONE', *, *, #6903, .F. ) ;
#3923 = CIRCLE ( 'NONE', #5498, 7.500000000000007105 ) ;
#3924 = CARTESIAN_POINT ( 'NONE',  ( -384.1454913942860685, 89.85401471197820911, -106.2499034276999055 ) ) ;
#3925 = EDGE_LOOP ( 'NONE', ( #3128, #5014 ) ) ;
#3926 = CARTESIAN_POINT ( 'NONE',  ( -820.7761598878998939, 74.70052632655239222, -154.6666544911500694 ) ) ;
#3927 = EDGE_LOOP ( 'NONE', ( #3676, #315, #2634, #4068 ) ) ;
#3928 = AXIS2_PLACEMENT_3D ( 'NONE', #285, #7711, #1173 ) ;
#3929 = APPLICATION_PROTOCOL_DEFINITION ( 'draft international standard', 'automotive_design', 1998, #2343 ) ;
#3930 = ORIENTED_EDGE ( 'NONE', *, *, #3053, .T. ) ;
#3931 = CARTESIAN_POINT ( 'NONE',  ( -954.5446161821273563, 49.54000128949434867, -118.7903414690681103 ) ) ;
#3932 = DIRECTION ( 'NONE',  ( -0.000000000000000000, -1.000000000000000000, -0.000000000000000000 ) ) ;
#3933 = CARTESIAN_POINT ( 'NONE',  ( -59.99999999999998579, -9.213203435596451385, -126.4213562373090696 ) ) ;
#3934 = CARTESIAN_POINT ( 'NONE',  ( 0.000000000000000000, -6.000000000000000000, 0.000000000000000000 ) ) ;
#3935 = AXIS2_PLACEMENT_3D ( 'NONE', #292, #1059, #4818 ) ;
#3936 = CARTESIAN_POINT ( 'NONE',  ( -904.1167769183953169, 122.8348148996191611, -113.1262384684093263 ) ) ;
#3937 = DIRECTION ( 'NONE',  ( -0.000000000000000000, -1.000000000000000000, -1.757987137413040192E-14 ) ) ;
#3938 = EDGE_LOOP ( 'NONE', ( #2981, #3105 ) ) ;
#3939 = CARTESIAN_POINT ( 'NONE',  ( -818.8285638327242850, 78.67432280806571043, -264.6807709998050200 ) ) ;
#3940 = ORIENTED_EDGE ( 'NONE', *, *, #7922, .T. ) ;
#3941 = CARTESIAN_POINT ( 'NONE',  ( -1019.365209469143679, 93.24061105504411273, -95.06748246948018277 ) ) ;
#3942 = MANIFOLD_SOLID_BREP ( 'Fillet8', #1973 ) ;
#3943 = CARTESIAN_POINT ( 'NONE',  ( -1011.051362836436624, 118.1813008219153716, -136.2353035311982126 ) ) ;
#3944 = LINE ( 'NONE', #2959, #4523 ) ;
#3945 = EDGE_CURVE ( 'NONE', #7284, #4621, #7893, .T. ) ;
#3946 = LINE ( 'NONE', #5736, #2428 ) ;
#3947 = ORIENTED_EDGE ( 'NONE', *, *, #4181, .T. ) ;
#3948 = DIRECTION ( 'NONE',  ( 0.000000000000000000, 1.000000000000000000, 0.000000000000000000 ) ) ;
#3949 = CARTESIAN_POINT ( 'NONE',  ( -818.8602300167369776, 79.32305858693273137, -104.8581405595891169 ) ) ;
#3950 = CARTESIAN_POINT ( 'NONE',  ( -144.0488662551579182, 12.00000000000000000, -146.9077238332691877 ) ) ;
#3951 = CARTESIAN_POINT ( 'NONE',  ( -1065.000000000002501, 109.8950841424301359, -136.2353035311980136 ) ) ;
#3952 = CARTESIAN_POINT ( 'NONE',  ( -380.5110847637466804, 99.61677185140682411, -115.1901175520814462 ) ) ;
#3953 = CARTESIAN_POINT ( 'NONE',  ( 0.000000000000000000, 0.000000000000000000, -89.68077099980401101 ) ) ;
#3954 = ORIENTED_EDGE ( 'NONE', *, *, #3181, .T. ) ;
#3955 = DIRECTION ( 'NONE',  ( -1.000000000000000000, 0.000000000000000000, 0.000000000000000000 ) ) ;
#3956 = CARTESIAN_POINT ( 'NONE',  ( 19.96040119434836768, 182.2179960502109850, -123.4119521547231386 ) ) ;
#3957 = CARTESIAN_POINT ( 'NONE',  ( -1014.632462699976486, 105.5176738732105690, -149.7857175106636589 ) ) ;
#3958 = FACE_BOUND ( 'NONE', #4353, .T. ) ;
#3959 = EDGE_CURVE ( 'NONE', #10867, #6680, #114, .T. ) ;
#3960 = ORIENTED_EDGE ( 'NONE', *, *, #10605, .F. ) ;
#3961 = ORIENTED_EDGE ( 'NONE', *, *, #1794, .F. ) ;
#3962 = CARTESIAN_POINT ( 'NONE',  ( 6.899999999999999467, 5.196152422706624030, -9.000000000000000000 ) ) ;
#3963 = CARTESIAN_POINT ( 'NONE',  ( -381.1761140529453087, 98.29529414878385296, -136.2909970179879906 ) ) ;
#3964 = DIRECTION ( 'NONE',  ( 0.000000000000000000, 1.000000000000000000, -0.000000000000000000 ) ) ;
#3965 = CARTESIAN_POINT ( 'NONE',  ( -902.4158961391586899, 71.79205886009079052, -149.7857175106635736 ) ) ;
#3966 = ORIENTED_EDGE ( 'NONE', *, *, #2818, .F. ) ;
#3967 = CARTESIAN_POINT ( 'NONE',  ( -374.7894439079065023, 75.48283603055834590, -143.6333451466693134 ) ) ;
#3968 = CARTESIAN_POINT ( 'NONE',  ( -370.4431240880636551, 57.15653990293812825, -114.9924028573050663 ) ) ;
#3969 = CARTESIAN_POINT ( 'NONE',  ( -374.9521586694311850, 79.37652290581388570, -94.82683079494582046 ) ) ;
#3970 = DIRECTION ( 'NONE',  ( 1.000000000000000000, 0.000000000000000000, 0.000000000000000000 ) ) ;
#3971 = VERTEX_POINT ( 'NONE', #5798 ) ;
#3972 = AXIS2_PLACEMENT_3D ( 'NONE', #11664, #8069, #1510 ) ;
#3973 = ORIENTED_EDGE ( 'NONE', *, *, #6074, .T. ) ;
#3974 = PRODUCT_DEFINITION_SHAPE ( 'NONE', 'NONE',  #12242 ) ;
#3975 = ORIENTED_EDGE ( 'NONE', *, *, #5169, .F. ) ;
#3976 = EDGE_CURVE ( 'NONE', #3716, #1640, #9463, .T. ) ;
#3977 = LINE ( 'NONE', #11585, #929 ) ;
#3978 = EDGE_CURVE ( 'NONE', #6402, #8803, #376, .T. ) ;
#3979 = CARTESIAN_POINT ( 'NONE',  ( -928.2641150402301946, 65.00826535581501275, -107.9061927053325576 ) ) ;
#3980 = CARTESIAN_POINT ( 'NONE',  ( -826.0484035456470338, 83.16661265238063550, -104.7144245788475558 ) ) ;
#3981 = CARTESIAN_POINT ( 'NONE',  ( 9.371890508914830252E-13, 0.000000000000000000, -36.42135623730949590 ) ) ;
#3982 = MANIFOLD_SOLID_BREP ( 'Fillet6', #4544 ) ;
#3983 = EDGE_LOOP ( 'NONE', ( #3301, #536 ) ) ;
#3984 = DIRECTION ( 'NONE',  ( 0.000000000000000000, 0.000000000000000000, -1.000000000000000000 ) ) ;
#3985 = EDGE_LOOP ( 'NONE', ( #7495, #685, #4363, #6562 ) ) ;
#3986 = CARTESIAN_POINT ( 'NONE',  ( -828.3859444281002880, 76.61103737358284604, -154.6660282174712222 ) ) ;
#3987 = VERTEX_POINT ( 'NONE', #4993 ) ;
#3988 = EDGE_CURVE ( 'NONE', #2611, #3899, #9271, .T. ) ;
#3989 = PRODUCT_CONTEXT ( 'NONE', #11196, 'mechanical' ) ;
#3990 = ORIENTED_EDGE ( 'NONE', *, *, #1560, .F. ) ;
#3991 = VECTOR ( 'NONE', #5112, 1000.000000000000000 ) ;
#3992 = CARTESIAN_POINT ( 'NONE',  ( -1025.806732200646138, 55.05754055295012961, -113.1262384684095537 ) ) ;
#3993 = DIRECTION ( 'NONE',  ( 0.000000000000000000, -1.156482317317870246E-16, 1.000000000000000000 ) ) ;
#3994 = CYLINDRICAL_SURFACE ( 'NONE', #11547, 1.500000000000000444 ) ;
#3995 = EDGE_CURVE ( 'NONE', #1396, #6687, #6172, .T. ) ;
#3996 = CARTESIAN_POINT ( 'NONE',  ( -1022.124201078493229, 113.7707856953083478, -107.9061927053324013 ) ) ;
#3997 = CARTESIAN_POINT ( 'NONE',  ( -818.8285638327206470, 78.34163520102097777, -105.0153140909395120 ) ) ;
#3998 = CARTESIAN_POINT ( 'NONE',  ( -19.92650117820961952, 178.2666534087950367, -126.3986386542856337 ) ) ;
#3999 = CARTESIAN_POINT ( 'NONE',  ( -112.4999999999999716, -9.213203435596451385, -126.4213562373086575 ) ) ;
#4000 = AXIS2_PLACEMENT_3D ( 'NONE', #8837, #10865, #3206 ) ;
#4001 = ORIENTED_EDGE ( 'NONE', *, *, #10401, .F. ) ;
#4002 = ORIENTED_EDGE ( 'NONE', *, *, #12140, .T. ) ;
#4003 = CARTESIAN_POINT ( 'NONE',  ( -952.1456544189251190, 108.1568929870907141, -99.57582448894486049 ) ) ;
#4004 = APPLICATION_CONTEXT ( 'automotive_design' ) ;
#4005 = ORIENTED_EDGE ( 'NONE', *, *, #8930, .T. ) ;
#4006 = CARTESIAN_POINT ( 'NONE',  ( -1060.773655115453948, 112.4236047030759238, -130.5712005305406080 ) ) ;
#4007 = DIRECTION ( 'NONE',  ( -1.000000000000000000, 0.000000000000000000, 0.000000000000000000 ) ) ;
#4008 = AXIS2_PLACEMENT_3D ( 'NONE', #2251, #10833, #6020 ) ;
#4009 = B_SPLINE_CURVE_WITH_KNOTS ( 'NONE', 3,
 ( #8241, #8582, #4753, #106, #3882, #7652, #2958, #8308 ),
 .UNSPECIFIED., .F., .F.,
 ( 4, 2, 2, 4 ),
 ( 0.005257893453559894098, 0.006567392922673226906, 0.007876892391786559713, 0.01049589133001322706 ),
 .UNSPECIFIED. ) ;
#4010 = CARTESIAN_POINT ( 'NONE',  ( -1021.743962174751232, 119.2557508373789403, -122.7172756069789585 ) ) ;
#4011 = EDGE_LOOP ( 'NONE', ( #2850, #4469, #11180, #7431 ) ) ;
#4012 = DIRECTION ( 'NONE',  ( -0.000000000000000000, 1.000000000000000000, 7.930164461608263644E-17 ) ) ;
#4013 = CIRCLE ( 'NONE', #5190, 10.00000000000000000 ) ;
#4014 = DIRECTION ( 'NONE',  ( 0.000000000000000000, 0.000000000000000000, 1.000000000000000000 ) ) ;
#4015 = FACE_OUTER_BOUND ( 'NONE', #7902, .T. ) ;
#4016 = CARTESIAN_POINT ( 'NONE',  ( -926.6866529579010603, 120.3119365386823034, -141.4553492942759760 ) ) ;
#4017 = DIRECTION ( 'NONE',  ( 0.000000000000000000, 0.000000000000000000, 1.000000000000000000 ) ) ;
#4018 = FACE_BOUND ( 'NONE', #6526, .T. ) ;
#4019 = VERTEX_POINT ( 'NONE', #295 ) ;
#4020 = CARTESIAN_POINT ( 'NONE',  ( -991.5701548301635739, 122.8678427087061493, -126.6442663926292056 ) ) ;
#4021 = LINE ( 'NONE', #301, #1222 ) ;
#4022 = CARTESIAN_POINT ( 'NONE',  ( -1025.044148074459827, 113.2108726315406813, -141.4553492942762318 ) ) ;
#4023 = CARTESIAN_POINT ( 'NONE',  ( -373.4475746528857485, 67.29758586747009019, -99.77979850356791758 ) ) ;
#4024 = VECTOR ( 'NONE', #1889, 1000.000000000000000 ) ;
#4025 = DIRECTION ( 'NONE',  ( 0.000000000000000000, 1.000000000000000000, 0.000000000000000000 ) ) ;
#4026 = ORIENTED_EDGE ( 'NONE', *, *, #9780, .T. ) ;
#4027 = ORIENTED_EDGE ( 'NONE', *, *, #8998, .F. ) ;
#4028 = CARTESIAN_POINT ( 'NONE',  ( -384.0282500477451322, 90.36076542521846022, -142.8872781659942177 ) ) ;
#4029 = DIRECTION ( 'NONE',  ( 0.000000000000000000, 0.000000000000000000, 1.000000000000000000 ) ) ;
#4030 = CARTESIAN_POINT ( 'NONE',  ( -956.9243412622475944, 54.10650223846812423, -141.4553492942761181 ) ) ;
#4031 = DIRECTION ( 'NONE',  ( 1.186840563529527301E-16, -1.000000000000000000, 0.000000000000000000 ) ) ;
#4032 = AXIS2_PLACEMENT_3D ( 'NONE', #1512, #8015, #516 ) ;
#4033 = EDGE_CURVE ( 'NONE', #5323, #9863, #7092, .T. ) ;
#4034 = CIRCLE ( 'NONE', #1274, 7.500000000000012434 ) ;
#4035 = CARTESIAN_POINT ( 'NONE',  ( -374.9975296411568024, 81.20712878759192677, -144.6676090229494775 ) ) ;
#4036 = DIRECTION ( 'NONE',  ( 0.9501779778103313090, 0.000000000000000000, -0.3117078928809301486 ) ) ;
#4037 = EDGE_CURVE ( 'NONE', #7759, #505, #574, .T. ) ;
#4038 = FACE_OUTER_BOUND ( 'NONE', #6376, .T. ) ;
#4039 = ORIENTED_EDGE ( 'NONE', *, *, #6516, .T. ) ;
#4040 = CARTESIAN_POINT ( 'NONE',  ( -1038.664246639927342, 43.28664065472985811, -136.2353035311990084 ) ) ;
#4041 = CARTESIAN_POINT ( 'NONE',  ( 45.00000000000001421, 25.00000000000002132, -126.4213562373094959 ) ) ;
#4042 = AXIS2_PLACEMENT_3D ( 'NONE', #12005, #8970, #8904 ) ;
#4043 = ORIENTED_EDGE ( 'NONE', *, *, #789, .T. ) ;
#4044 = ADVANCED_FACE ( 'NONE', ( #5985 ), #8032, .F. ) ;
#4045 = CIRCLE ( 'NONE', #895, 81.99999999999998579 ) ;
#4046 = CARTESIAN_POINT ( 'NONE',  ( 19.99813415626286783, 177.7525720880900053, -124.3666714923229222 ) ) ;
#4047 = CARTESIAN_POINT ( 'NONE',  ( -901.9718911164643487, 59.00785292138902349, -113.1262384684096105 ) ) ;
#4048 = DIRECTION ( 'NONE',  ( -0.000000000000000000, -0.000000000000000000, -1.000000000000000000 ) ) ;
#4049 = ORIENTED_EDGE ( 'NONE', *, *, #6369, .T. ) ;
#4050 = ORIENTED_EDGE ( 'NONE', *, *, #3945, .T. ) ;
#4051 = DIRECTION ( 'NONE',  ( 1.000000000000000000, 1.186840563529527301E-16, 0.000000000000000000 ) ) ;
#4052 = VERTEX_POINT ( 'NONE', #4141 ) ;
#4053 = CIRCLE ( 'NONE', #1886, 134.9999999999999716 ) ;
#4054 = SHAPE_DEFINITION_REPRESENTATION ( #6054, #6213 ) ;
#4055 = AXIS2_PLACEMENT_3D ( 'NONE', #556, #618, #2474 ) ;
#4056 = ORIENTED_EDGE ( 'NONE', *, *, #6479, .T. ) ;
#4057 = CARTESIAN_POINT ( 'NONE',  ( -1057.832023714519210, 42.29985473022490794, -122.7172756069794559 ) ) ;
#4058 = EDGE_CURVE ( 'NONE', #7697, #6496, #469, .T. ) ;
#4059 = CARTESIAN_POINT ( 'NONE',  ( 9.184850993605153861E-16, -6.000000000000000000, -133.9213562373095101 ) ) ;
#4060 = CYLINDRICAL_SURFACE ( 'NONE', #7553, 7.500000000000007105 ) ;
#4061 = PRODUCT_RELATED_PRODUCT_CATEGORY ( 'part', '', ( #2792 ) ) ;
#4062 = TOROIDAL_SURFACE ( 'NONE', #2677, 44.00000000000000711, 1.000000000000000000 ) ;
#4063 = CARTESIAN_POINT ( 'NONE',  ( -1014.382386707157252, 110.5980896718282196, -103.3307627799636350 ) ) ;
#4064 = DIRECTION ( 'NONE',  ( 0.000000000000000000, -1.156482317317870246E-16, 1.000000000000000000 ) ) ;
#4065 = CARTESIAN_POINT ( 'NONE',  ( -19.98030737385957423, 179.4757119253121402, -125.9751133749524712 ) ) ;
#4066 = ORIENTED_EDGE ( 'NONE', *, *, #11821, .F. ) ;
#4067 = DIRECTION ( 'NONE',  ( 0.000000000000000000, 1.000000000000000000, 6.938893903907169213E-16 ) ) ;
#4068 = ORIENTED_EDGE ( 'NONE', *, *, #8952, .F. ) ;
#4069 = CARTESIAN_POINT ( 'NONE',  ( -1011.662592067698938, 105.4443429699071828, -99.57582448894505944 ) ) ;
#4070 = EDGE_CURVE ( 'NONE', #5809, #140, #7211, .T. ) ;
#4071 = ORIENTED_EDGE ( 'NONE', *, *, #4965, .T. ) ;
#4072 = CARTESIAN_POINT ( 'NONE',  ( -991.6207251904210125, 122.2801902404846714, -130.5712005305406080 ) ) ;
#4073 = FACE_OUTER_BOUND ( 'NONE', #1930, .T. ) ;
#4074 = CARTESIAN_POINT ( 'NONE',  ( 19.95569904651928184, 178.2465785626148431, -123.3391210327002199 ) ) ;
#4075 = CARTESIAN_POINT ( 'NONE',  ( -991.6207251904191935, 122.2801902404845151, -118.7903414690677124 ) ) ;
#4076 = ORIENTED_EDGE ( 'NONE', *, *, #5169, .T. ) ;
#4077 = CARTESIAN_POINT ( 'NONE',  ( 1.249585401188644101E-12, 164.0000000000000000, -6.421356237309481685 ) ) ;
#4078 = CARTESIAN_POINT ( 'NONE',  ( -822.0624079427799415, 83.35484814232630413, -104.7266156443419050 ) ) ;
#4079 = CARTESIAN_POINT ( 'NONE',  ( 1.734723475976807094E-15, 180.2041921146324910, -179.7948474705909234 ) ) ;
#4080 = VECTOR ( 'NONE', #381, 1000.000000000000000 ) ;
#4081 =( NAMED_UNIT ( * ) SI_UNIT ( $, .STERADIAN. ) SOLID_ANGLE_UNIT ( ) );
#4082 = FACE_BOUND ( 'NONE', #9321, .T. ) ;
#4083 = ORIENTED_EDGE ( 'NONE', *, *, #1726, .F. ) ;
#4084 = CARTESIAN_POINT ( 'NONE',  ( 2.186774452080127126E-12, 12.00000000000000000, 83.57864376269050410 ) ) ;
#4085 = DIRECTION ( 'NONE',  ( 0.000000000000000000, 0.000000000000000000, -1.000000000000000000 ) ) ;
#4086 = PRODUCT_DEFINITION_SHAPE ( 'NONE', 'NONE',  #12247 ) ;
#4087 = CARTESIAN_POINT ( 'NONE',  ( -144.0488662551579182, 0.000000000000000000, -146.9077238332691877 ) ) ;
#4088 = CARTESIAN_POINT ( 'NONE',  ( -1018.154501869017849, 114.3413228342528214, -141.4553492942762887 ) ) ;
#4089 = FACE_OUTER_BOUND ( 'NONE', #5677, .T. ) ;
#4090 = VERTEX_POINT ( 'NONE', #7003 ) ;
#4091 = AXIS2_PLACEMENT_3D ( 'NONE', #12015, #8390, #1694 ) ;
#4092 = LINE ( 'NONE', #7861, #10009 ) ;
#4093 = ORIENTED_EDGE ( 'NONE', *, *, #10852, .T. ) ;
#4094 = CARTESIAN_POINT ( 'NONE',  ( -382.6758974726718634, 94.76977496699193182, -140.0841047258399215 ) ) ;
#4095 = CARTESIAN_POINT ( 'NONE',  ( -818.6751755801125228, 47.70925804672287995, -149.7857175106634884 ) ) ;
#4096 = CARTESIAN_POINT ( 'NONE',  ( 1.875296586882326249E-12, 163.9999999999999716, 46.07864376269051121 ) ) ;
#4097 = CARTESIAN_POINT ( 'NONE',  ( -29.03136272649514638, 180.2041921146316668, -134.6807709998038547 ) ) ;
#4098 = CARTESIAN_POINT ( 'NONE',  ( -380.4977426702656658, 64.35709158751954817, -115.2383737207536427 ) ) ;
#4099 = CARTESIAN_POINT ( 'NONE',  ( -825.1267440042464614, 73.83480927677597094, -94.70504551274875382 ) ) ;
#4100 = AXIS2_PLACEMENT_3D ( 'NONE', #11786, #3306, #9182 ) ;
#4101 = CARTESIAN_POINT ( 'NONE',  ( -1048.334963668468163, 42.40858384259928471, -136.2353035311987242 ) ) ;
#4102 = EDGE_LOOP ( 'NONE', ( #9049, #7363 ) ) ;
#4103 = ADVANCED_FACE ( 'NONE', ( #6200 ), #323, .F. ) ;
#4104 = CIRCLE ( 'NONE', #3302, 69.99999999999998579 ) ;
#4105 = CARTESIAN_POINT ( 'NONE',  ( -954.4431216459856842, 51.77564274757639140, -113.1262384684095537 ) ) ;
#4106 = CARTESIAN_POINT ( 'NONE',  ( -19.87821795393918478, 180.7372106301276062, -122.4761893939201940 ) ) ;
#4107 = CARTESIAN_POINT ( 'NONE',  ( 126.4213562373094959, 12.00000000000000000, 7.500000000000007105 ) ) ;
#4108 = ORIENTED_EDGE ( 'NONE', *, *, #8375, .F. ) ;
#4109 = CARTESIAN_POINT ( 'NONE',  ( -828.3857845960920940, 80.73794319005740761, -94.93252152554778434 ) ) ;
#4110 = CARTESIAN_POINT ( 'NONE',  ( -381.1875678672224694, 65.72850031932472348, -113.0372152455248198 ) ) ;
#4111 = ORIENTED_EDGE ( 'NONE', *, *, #4280, .T. ) ;
#4112 = CARTESIAN_POINT ( 'NONE',  ( -827.1306228376723766, 74.90530319234137835, -154.6796240013121064 ) ) ;
#4113 = ORIENTED_EDGE ( 'NONE', *, *, #8375, .T. ) ;
#4114 = ITEM_DEFINED_TRANSFORMATION ( 'NONE', 'NONE', #8217,  #11957 ) ;
#4115 = ORIENTED_EDGE ( 'NONE', *, *, #5783, .T. ) ;
#4116 = CARTESIAN_POINT ( 'NONE',  ( -1057.805062346511704, 42.77845103615958067, -118.7903414690684087 ) ) ;
#4117 = CARTESIAN_POINT ( 'NONE',  ( -180.0000000000000000, -9.213203435596478030, -126.4213562373082453 ) ) ;
#4118 = CARTESIAN_POINT ( 'NONE',  ( 1.249585401188644101E-12, 12.00000000000000000, -6.421356237309494119 ) ) ;
#4119 = EDGE_CURVE ( 'NONE', #10573, #6737, #1189, .T. ) ;
#4120 = AXIS2_PLACEMENT_3D ( 'NONE', #2505, #7209, #7399 ) ;
#4121 = CARTESIAN_POINT ( 'NONE',  ( -926.8105964072291272, 116.1567348237266515, -103.3307627799635213 ) ) ;
#4122 = DIRECTION ( 'NONE',  ( 0.000000000000000000, 0.000000000000000000, 1.000000000000000000 ) ) ;
#4123 = EDGE_CURVE ( 'NONE', #3186, #1611, #8088, .T. ) ;
#4124 = ORIENTED_EDGE ( 'NONE', *, *, #6843, .F. ) ;
#4125 = VERTEX_POINT ( 'NONE', #4350 ) ;
#4126 = CARTESIAN_POINT ( 'NONE',  ( -1031.476138302181198, 95.34216976508436403, -96.78565065507929432 ) ) ;
#4127 = CIRCLE ( 'NONE', #8284, 7.500000000000007105 ) ;
#4128 = CARTESIAN_POINT ( 'NONE',  ( -1013.875822516560447, 120.2710389253235519, -124.6807709998039257 ) ) ;
#4129 = DIRECTION ( 'NONE',  ( -1.000000000000000000, 0.000000000000000000, 0.000000000000000000 ) ) ;
#4130 = CARTESIAN_POINT ( 'NONE',  ( 19.98454104437637824, 177.9140520261175311, -123.8699308089654778 ) ) ;
#4131 = AXIS2_PLACEMENT_3D ( 'NONE', #12123, #993, #3634 ) ;
#4132 = EDGE_LOOP ( 'NONE', ( #2816, #9607 ) ) ;
#4133 = EDGE_CURVE ( 'NONE', #9567, #11989, #7063, .T. ) ;
#4134 = CARTESIAN_POINT ( 'NONE',  ( -819.0908526083424022, 77.06787236046197620, -144.0637517540454553 ) ) ;
#4135 = ADVANCED_FACE ( 'NONE', ( #1325 ), #286, .F. ) ;
#4136 = CIRCLE ( 'NONE', #10644, 7.500000000000007105 ) ;
#4137 = DIRECTION ( 'NONE',  ( 0.000000000000000000, 0.000000000000000000, 1.000000000000000000 ) ) ;
#4138 = CARTESIAN_POINT ( 'NONE',  ( -1017.158871447982392, 53.64146012065780411, -124.6807709998041389 ) ) ;
#4139 = CIRCLE ( 'NONE', #983, 1.499999999999998224 ) ;
#4140 = CARTESIAN_POINT ( 'NONE',  ( -372.8331336047301079, 100.5030287243513385, -117.0268099732259515 ) ) ;
#4141 = CARTESIAN_POINT ( 'NONE',  ( 9.371890508914830252E-13, 164.0000000000000000, -28.92135623730947458 ) ) ;
#4142 = FACE_BOUND ( 'NONE', #10523, .T. ) ;
#4143 = EDGE_LOOP ( 'NONE', ( #10187, #3400 ) ) ;
#4144 = CARTESIAN_POINT ( 'NONE',  ( -955.0000000000038654, 82.00000000000036948, -124.6807709998041673 ) ) ;
#4145 = CARTESIAN_POINT ( 'NONE',  ( -1021.743962174751232, 119.2557508373790824, -126.6442663926290209 ) ) ;
#4146 = CARTESIAN_POINT ( 'NONE',  ( 0.000000000000000000, 12.00000000000000000, -124.6807709998040110 ) ) ;
#4147 = CARTESIAN_POINT ( 'NONE',  ( -126.4213562373094959, -494.9999999999998863, 2.255140518769849223E-14 ) ) ;
#4148 = ORIENTED_EDGE ( 'NONE', *, *, #8792, .F. ) ;
#4149 = ORIENTED_EDGE ( 'NONE', *, *, #11461, .T. ) ;
#4150 = DIRECTION ( 'NONE',  ( -8.163404592832031500E-17, 1.000000000000000000, 0.000000000000000000 ) ) ;
#4151 = CARTESIAN_POINT ( 'NONE',  ( -383.8834587150378184, 73.10403131824993750, -142.6030770266003742 ) ) ;
#4152 = CARTESIAN_POINT ( 'NONE',  ( 20.00000000000000000, 196.0000000000000000, -124.6807709998038405 ) ) ;
#4153 = CARTESIAN_POINT ( 'NONE',  ( -375.0000000000000568, 83.44897642188486486, -154.6807709998038831 ) ) ;
#4154 = DIRECTION ( 'NONE',  ( 1.000000000000000000, 0.000000000000000000, 0.000000000000000000 ) ) ;
#4155 = CARTESIAN_POINT ( 'NONE',  ( -141.4213562373095101, -6.000000000000000000, 3.644282033693712520E-14 ) ) ;
#4156 = DIRECTION ( 'NONE',  ( -0.000000000000000000, -1.000000000000000000, -0.000000000000000000 ) ) ;
#4157 = CARTESIAN_POINT ( 'NONE',  ( -818.1708872189602744, 40.82851623284160070, -146.0307792196448702 ) ) ;
#4158 =( BOUNDED_SURFACE ( )  B_SPLINE_SURFACE ( 3, 2, ( 
 ( #10886, #8969, #3582 ),
 ( #5259, #9027, #7372 ),
 ( #567, #2670, #6444 ),
 ( #3524, #4348, #10087 ),
 ( #11146, #3460, #7315 ),
 ( #4538, #1620, #6378 ),
 ( #2545, #8115, #10954 ),
 ( #9090, #497, #2417 ),
 ( #5443, #4402, #2483 ),
 ( #11880, #6259, #10028 ),
 ( #11943, #1555, #630 ),
 ( #6318, #5377, #9221 ),
 ( #8314, #9156, #4470 ),
 ( #12074, #9290, #2978 ),
 ( #1934, #2799, #11384 ),
 ( #4722, #4603, #4665 ),
 ( #11212, #5697, #2737 ),
 ( #9469, #3843, #4829 ),
 ( #6504, #1814, #8443 ),
 ( #9528, #11447, #127 ),
 ( #1009, #894, #7618 ),
 ( #830, #1995, #5578 ),
 ( #8374, #6568, #10460 ),
 ( #3903, #9351, #12202 ),
 ( #3722, #7676, #1876 ),
 ( #8497, #3080, #162 ),
 ( #1912, #4755, #3886 ),
 ( #5676, #11378, #44 ) ),
 .UNSPECIFIED., .F., .F., .F. ) 
 B_SPLINE_SURFACE_WITH_KNOTS ( ( 4, 2, 2, 2, 2, 2, 2, 2, 2, 2, 2, 2, 2, 4 ),
 ( 3, 3 ),
 ( 0.000000000000000000, 0.0004930383923902153772, 0.0009860767847804307543, 0.001479115177170646240, 0.001972153569560861509, 0.002958230354341292480, 0.003451268746731507749, 0.003944307139121723017, 0.004437345531511939153, 0.004930383923902154422, 0.005916460708682584960, 0.006409499101072800228, 0.006902537493463015497, 0.007888614278243446035 ),
 ( 0.000000000000000000, 1.000000000000000000 ),
 .UNSPECIFIED. ) 
 GEOMETRIC_REPRESENTATION_ITEM ( )  RATIONAL_B_SPLINE_SURFACE ( (
 ( 1.000000000000000000, 0.6689879873414465994, 1.000000000000000000),
 ( 1.000000000000000000, 0.6682619615833934601, 1.000000000000000000),
 ( 1.000000000000000000, 0.6677734440439352381, 1.000000000000000000),
 ( 1.000000000000000000, 0.6670763045104984856, 1.000000000000000000),
 ( 1.000000000000000000, 0.6668655740656856956, 1.000000000000000000),
 ( 1.000000000000000000, 0.6666182310250359233, 1.000000000000000000),
 ( 1.000000000000000000, 0.6665784742421086984, 1.000000000000000000),
 ( 1.000000000000000000, 0.6666353228050939661, 1.000000000000000000),
 ( 1.000000000000000000, 0.6667346642862397310, 1.000000000000000000),
 ( 1.000000000000000000, 0.6673328464405002824, 1.000000000000000000),
 ( 1.000000000000000000, 0.6681342971656755170, 1.000000000000000000),
 ( 1.000000000000000000, 0.6708694338352457764, 1.000000000000000000),
 ( 1.000000000000000000, 0.6720569605147309611, 1.000000000000000000),
 ( 1.000000000000000000, 0.6751225054005377535, 1.000000000000000000),
 ( 1.000000000000000000, 0.6769812796920648967, 1.000000000000000000),
 ( 1.000000000000000000, 0.6815111439571803764, 1.000000000000000000),
 ( 1.000000000000000000, 0.6842124604620484218, 1.000000000000000000),
 ( 1.000000000000000000, 0.6903314890518940095, 1.000000000000000000),
 ( 1.000000000000000000, 0.6937642806658218531, 1.000000000000000000),
 ( 1.000000000000000000, 0.7052556801245680740, 1.000000000000000000),
 ( 1.000000000000000000, 0.7142546037275387949, 1.000000000000000000),
 ( 1.000000000000000000, 0.7287603549096577371, 1.000000000000000000),
 ( 1.000000000000000000, 0.7336520540315742966, 1.000000000000000000),
 ( 1.000000000000000000, 0.7434275992171806013, 1.000000000000000000),
 ( 1.000000000000000000, 0.7483638594814020495, 1.000000000000000000),
 ( 1.000000000000000000, 0.7624769318894530912, 1.000000000000000000),
 ( 1.000000000000000000, 0.7710581372201869010, 1.000000000000000000),
 ( 1.000000000000000000, 0.7778924984312529656, 1.000000000000000000) ) ) 
 REPRESENTATION_ITEM ( '' )  SURFACE ( )  );
#4159 = ORIENTED_EDGE ( 'NONE', *, *, #8755, .T. ) ;
#4160 = ORIENTED_EDGE ( 'NONE', *, *, #6087, .F. ) ;
#4161 = DIRECTION ( 'NONE',  ( 0.000000000000000000, 1.000000000000000000, 0.000000000000000000 ) ) ;
#4162 = CARTESIAN_POINT ( 'NONE',  ( -1032.644706488208840, 45.21923725197571997, -118.7903414690683519 ) ) ;
#4163 = ORIENTED_EDGE ( 'NONE', *, *, #11692, .T. ) ;
#4164 = CARTESIAN_POINT ( 'NONE',  ( -825.1270161104789622, 83.51388719778367431, -95.24185468551783629 ) ) ;
#4165 = CARTESIAN_POINT ( 'NONE',  ( -381.0136216353810141, 98.62943157718950715, -113.5542780775817420 ) ) ;
#4166 = CARTESIAN_POINT ( 'NONE',  ( -828.8285638327247398, 78.67432280806576728, -154.5823979888776591 ) ) ;
#4167 = ORIENTED_EDGE ( 'NONE', *, *, #4362, .F. ) ;
#4168 = ADVANCED_FACE ( 'NONE', ( #11499 ), #117, .F. ) ;
#4169 = EDGE_LOOP ( 'NONE', ( #10008, #9035, #7816, #11194 ) ) ;
#4170 = CARTESIAN_POINT ( 'NONE',  ( -1021.483947769352199, 56.15424078096101113, -113.1262384684096105 ) ) ;
#4171 = CARTESIAN_POINT ( 'NONE',  ( -21.06240745282767080, 180.2041921146517041, -126.4269926335259413 ) ) ;
#4172 = CARTESIAN_POINT ( 'NONE',  ( -1023.078931369429029, 98.73915068298381925, -96.78565065507928011 ) ) ;
#4173 = DIRECTION ( 'NONE',  ( 0.000000000000000000, 0.000000000000000000, -1.000000000000000000 ) ) ;
#4174 = ORIENTED_EDGE ( 'NONE', *, *, #7577, .F. ) ;
#4175 = DIRECTION ( 'NONE',  ( 0.000000000000000000, -1.156482317317870246E-16, 1.000000000000000000 ) ) ;
#4176 =( LENGTH_UNIT ( ) NAMED_UNIT ( * ) SI_UNIT ( .MILLI., .METRE. ) );
#4177 = VECTOR ( 'NONE', #3260, 1000.000000000000000 ) ;
#4178 = EDGE_CURVE ( 'NONE', #10083, #6648, #11019, .T. ) ;
#4179 = ORIENTED_EDGE ( 'NONE', *, *, #5104, .T. ) ;
#4181 = EDGE_CURVE ( 'NONE', #4517, #6610, #3522, .T. ) ;
#4180 = CARTESIAN_POINT ( 'NONE',  ( -974.7984820115178763, 96.63273410478059589, -96.78565065507896747 ) ) ;
#4182 = CARTESIAN_POINT ( 'NONE',  ( -28.53314250459843038, 180.2041921146317236, -137.7978499286131751 ) ) ;
#4183 = CARTESIAN_POINT ( 'NONE',  ( -1054.380968608929606, 114.0683136310380803, -126.6442663926291345 ) ) ;
#4184 = FACE_OUTER_BOUND ( 'NONE', #8438, .T. ) ;
#4185 = CARTESIAN_POINT ( 'NONE',  ( 19.88975813659335756, 181.1020309933168164, -122.5829583614533362 ) ) ;
#4186 = VECTOR ( 'NONE', #7163, 1000.000000000000000 ) ;
#4187 = ADVANCED_FACE ( 'NONE', ( #6039 ), #1401, .F. ) ;
#4188 = CARTESIAN_POINT ( 'NONE',  ( -1054.519145619997744, 111.4921997120089401, -113.1262384684101079 ) ) ;
#4189 = LINE ( 'NONE', #465, #3142 ) ;
#4190 = CARTESIAN_POINT ( 'NONE',  ( -19.99715534307563658, 182.6423572728569980, -124.2973801271140246 ) ) ;
#4191 = CARTESIAN_POINT ( 'NONE',  ( -826.3398728605874339, 83.01019204304883203, -104.7054730589233458 ) ) ;
#4192 = CARTESIAN_POINT ( 'NONE',  ( -1032.658196452834090, 44.72920460984212809, -124.6807709998042100 ) ) ;
#4193 = CARTESIAN_POINT ( 'NONE',  ( -370.5023963858000684, 106.6873030616109901, -114.4724351692933055 ) ) ;
#4194 = CARTESIAN_POINT ( 'NONE',  ( -818.8285638327246261, 79.00509885246378872, -94.75329546164918781 ) ) ;
#4195 = PLANE ( 'NONE',  #11765 ) ;
#4196 = EDGE_LOOP ( 'NONE', ( #5886, #2895, #6082, #829, #8818 ) ) ;
#4197 = CARTESIAN_POINT ( 'NONE',  ( -202.4999999999999716, 12.00000000000001421, -126.4213562373080180 ) ) ;
#4198 = CIRCLE ( 'NONE', #11706, 7.500000000000013323 ) ;
#4199 = CARTESIAN_POINT ( 'NONE',  ( -1021.743962174751232, 119.2557508373789403, -124.6807709998040110 ) ) ;
#4200 = CYLINDRICAL_SURFACE ( 'NONE', #10096, 7.500000000000007105 ) ;
#4201 = CARTESIAN_POINT ( 'NONE',  ( -374.3141123712231320, 72.20286621420174811, -96.83681641041877697 ) ) ;
#4202 = EDGE_CURVE ( 'NONE', #1329, #822, #6877, .T. ) ;
#4203 = DIRECTION ( 'NONE',  ( -8.163404592832030268E-17, 1.000000000000000000, -0.000000000000000000 ) ) ;
#4204 = ORIENTED_EDGE ( 'NONE', *, *, #5019, .F. ) ;
#4205 = CARTESIAN_POINT ( 'NONE',  ( 19.87222254682778910, 180.2228354577052301, -122.4235914049322389 ) ) ;
#4206 = ADVANCED_FACE ( 'NONE', ( #11789 ), #7023, .T. ) ;
#4207 = CARTESIAN_POINT ( 'NONE',  ( -383.7473746520292366, 72.58506784310948490, -142.3356691012474755 ) ) ;
#4208 = CARTESIAN_POINT ( 'NONE',  ( 2.510525938252074008E-14, -7.999999999999979572, -124.6807709998038405 ) ) ;
#4209 = CARTESIAN_POINT ( 'NONE',  ( -372.9446032145285699, 98.87496311769449164, -147.7124752337511779 ) ) ;
#4210 = FACE_OUTER_BOUND ( 'NONE', #10593, .T. ) ;
#4211 = CARTESIAN_POINT ( 'NONE',  ( -373.9258432311627303, 68.44287225057918533, -109.8786234846105998 ) ) ;
#4212 = CARTESIAN_POINT ( 'NONE',  ( -820.5263375362879970, 74.90579914177446597, -94.69102061099690104 ) ) ;
#4213 = CIRCLE ( 'NONE', #1254, 7.500000000000013323 ) ;
#4214 = ORIENTED_EDGE ( 'NONE', *, *, #11025, .F. ) ;
#4215 = CARTESIAN_POINT ( 'NONE',  ( -1025.000791045970800, 67.42844482392692385, -149.7857175106636305 ) ) ;
#4216 = EDGE_CURVE ( 'NONE', #8861, #5315, #8061, .T. ) ;
#4217 = ORIENTED_EDGE ( 'NONE', *, *, #4405, .T. ) ;
#4218 = AXIS2_PLACEMENT_3D ( 'NONE', #442, #2321, #9859 ) ;
#4219 = VECTOR ( 'NONE', #3707, 1000.000000000000000 ) ;
#4220 = CARTESIAN_POINT ( 'NONE',  ( -928.4218612484631876, 59.99049470396640515, -118.7903414690680535 ) ) ;
#4221 = CARTESIAN_POINT ( 'NONE',  ( 141.4213562373095101, -494.9999999999998863, -1.508194112741312283E-14 ) ) ;
#4222 = CARTESIAN_POINT ( 'NONE',  ( -825.4392429272181744, 83.41914585070148291, -95.23026386004784172 ) ) ;
#4223 = CARTESIAN_POINT ( 'NONE',  ( -305.0000000000000568, 11.99999999999998224, -159.6807709998038547 ) ) ;
#4224 = ORIENTED_EDGE ( 'NONE', *, *, #6619, .T. ) ;
#4225 = CARTESIAN_POINT ( 'NONE',  ( 8.500000000000008882, 166.0000000000000000, -124.6807709998038405 ) ) ;
#4226 = ORIENTED_EDGE ( 'NONE', *, *, #3270, .T. ) ;
#4227 = CARTESIAN_POINT ( 'NONE',  ( -795.0000000000036380, 52.00000000000027711, -126.6442663926292624 ) ) ;
#4228 = VECTOR ( 'NONE', #9157, 1000.000000000000000 ) ;
#4229 = AXIS2_PLACEMENT_3D ( 'NONE', #4097, #9018, #7927 ) ;
#4230 = CARTESIAN_POINT ( 'NONE',  ( 8.099999999999999645, 0.000000000000000000, 5.999999999999999112 ) ) ;
#4231 = CARTESIAN_POINT ( 'NONE',  ( 0.000000000000000000, -494.9999999999998863, -126.4213562373094959 ) ) ;
#4232 = CYLINDRICAL_SURFACE ( 'NONE', #11293, 5.999999999999999112 ) ;
#4233 = LINE ( 'NONE', #3294, #511 ) ;
#4234 = LINE ( 'NONE', #1020, #6782 ) ;
#4235 = APPLICATION_CONTEXT ( 'automotive_design' ) ;
#4236 = CARTESIAN_POINT ( 'NONE',  ( -927.1204550305436669, 105.3607176047075029, -96.78565065507918064 ) ) ;
#4237 = DIRECTION ( 'NONE',  ( 0.000000000000000000, 1.000000000000000000, 0.000000000000000000 ) ) ;
#4238 = CARTESIAN_POINT ( 'NONE',  ( -19.99263453218006603, 177.7304828429992654, -125.2341356145629732 ) ) ;
#4239 = AXIS2_PLACEMENT_3D ( 'NONE', #11561, #3303, #5162 ) ;
#4240 = EDGE_LOOP ( 'NONE', ( #3930, #12072 ) ) ;
#4241 = AXIS2_PLACEMENT_3D ( 'NONE', #10204, #11934, #10136 ) ;
#4242 = CARTESIAN_POINT ( 'NONE',  ( -379.7921418149276747, 63.07164944985365906, -118.2218589048162016 ) ) ;
#4243 = CARTESIAN_POINT ( 'NONE',  ( -374.9543748372134360, 85.20913091084348423, -104.9194821374490090 ) ) ;
#4244 = VERTEX_POINT ( 'NONE', #10914 ) ;
#4245 = CARTESIAN_POINT ( 'NONE',  ( 11.89695805161204234, 180.2041921146325762, -183.6976696918630125 ) ) ;
#4246 =( LENGTH_UNIT ( ) NAMED_UNIT ( * ) SI_UNIT ( .MILLI., .METRE. ) );
#4247 = DIRECTION ( 'NONE',  ( -1.000000000000000000, -0.000000000000000000, -0.000000000000000000 ) ) ;
#4248 = EDGE_LOOP ( 'NONE', ( #7773, #7279 ) ) ;
#4249 = CARTESIAN_POINT ( 'NONE',  ( -996.0013826475885708, 63.70094029248571132, -96.78565065507963538 ) ) ;
#4250 = B_SPLINE_CURVE_WITH_KNOTS ( 'NONE', 3,
 ( #8584, #9327, #3819, #1731, #1054, #108, #9509, #6604, #3884, #8350 ),
 .UNSPECIFIED., .F., .F.,
 ( 4, 2, 2, 2, 4 ),
 ( 0.01531771418541752645, 0.01599364935748912725, 0.01666958452956072631, 0.01734551970163232884, 0.01802145487370392790 ),
 .UNSPECIFIED. ) ;
#4251 = CARTESIAN_POINT ( 'NONE',  ( 19.92885329534479055, 181.8094058714599157, -122.9898942296876356 ) ) ;
#4252 = CARTESIAN_POINT ( 'NONE',  ( -20.94548197283593893, 181.6568612240360210, -124.4525847695740310 ) ) ;
#4253 = CARTESIAN_POINT ( 'NONE',  ( -823.8285638327238303, 78.67432280806536937, -89.68077099980398259 ) ) ;
#4254 = CARTESIAN_POINT ( 'NONE',  ( 19.97670222400810758, 180.3732814399037068, -126.1531159571454310 ) ) ;
#4255 = VECTOR ( 'NONE', #11323, 1000.000000000000000 ) ;
#4256 = CARTESIAN_POINT ( 'NONE',  ( 19.87445315872311369, 179.8633251070327219, -122.4428743481628601 ) ) ;
#4257 = CIRCLE ( 'NONE', #7402, 7.500000000000007105 ) ;
#4258 = EDGE_CURVE ( 'NONE', #11998, #8531, #2043, .T. ) ;
#4259 = CARTESIAN_POINT ( 'NONE',  ( 0.000000000000000000, 12.00000000000001776, -89.68077099980384048 ) ) ;
#4260 = EDGE_CURVE ( 'NONE', #7692, #481, #1952, .T. ) ;
#4261 = FACE_BOUND ( 'NONE', #8800, .T. ) ;
#4262 = DIRECTION ( 'NONE',  ( 0.000000000000000000, 1.000000000000000000, 0.000000000000000000 ) ) ;
#4263 = CARTESIAN_POINT ( 'NONE',  ( 35.00000000000000000, 139.9999999999999716, -89.68077099980384048 ) ) ;
#4264 = AXIS2_PLACEMENT_3D ( 'NONE', #1639, #5277, #9051 ) ;
#4265 = DIRECTION ( 'NONE',  ( -1.000000000000000000, 0.000000000000000000, -0.000000000000000000 ) ) ;
#4266 = EDGE_LOOP ( 'NONE', ( #2422, #4697, #5199, #3265 ) ) ;
#4267 = CARTESIAN_POINT ( 'NONE',  ( -7.499999999999996447, 12.00000000000001776, -126.4213562373094959 ) ) ;
#4268 = DIRECTION ( 'NONE',  ( 0.000000000000000000, 0.000000000000000000, -1.000000000000000000 ) ) ;
#4269 = EDGE_CURVE ( 'NONE', #481, #7692, #3310, .T. ) ;
#4270 = DIRECTION ( 'NONE',  ( 1.000000000000000000, 0.000000000000000000, -0.000000000000000000 ) ) ;
#4271 = DIRECTION ( 'NONE',  ( 0.000000000000000000, 0.000000000000000000, 1.000000000000000000 ) ) ;
#4272 = CYLINDRICAL_SURFACE ( 'NONE', #4971, 81.99999999999998579 ) ;
#4273 = EDGE_LOOP ( 'NONE', ( #6438, #1483 ) ) ;
#4274 = CIRCLE ( 'NONE', #932, 7.500000000000007105 ) ;
#4275 = CARTESIAN_POINT ( 'NONE',  ( 3.123963502971610252E-13, 164.0000000000000000, -96.42135623730948168 ) ) ;
#4276 = EDGE_CURVE ( 'NONE', #725, #739, #10233, .T. ) ;
#4277 = CARTESIAN_POINT ( 'NONE',  ( -371.9170445678053625, 102.5500601245914964, -143.3619720575524070 ) ) ;
#4278 = CARTESIAN_POINT ( 'NONE',  ( 0.07568653364411878637, -1.751902528157375682, 8.999999999999998224 ) ) ;
#4279 = LINE ( 'NONE', #5312, #5478 ) ;
#4280 = EDGE_CURVE ( 'NONE', #6415, #6258, #150, .T. ) ;
#4281 = CYLINDRICAL_SURFACE ( 'NONE', #6501, 69.99999999999995737 ) ;
#4282 = VERTEX_POINT ( 'NONE', #8081 ) ;
#4283 = CARTESIAN_POINT ( 'NONE',  ( -1013.392840968502924, 67.31954129910421614, -149.7857175106636873 ) ) ;
#4284 = AXIS2_PLACEMENT_3D ( 'NONE', #2320, #6089, #4357 ) ;
#4285 = VERTEX_POINT ( 'NONE', #8021 ) ;
#4286 = EDGE_LOOP ( 'NONE', ( #980, #9292, #2974, #3947, #2990, #7688, #4027, #6578, #9280, #3378 ) ) ;
#4287 = DIRECTION ( 'NONE',  ( -0.000000000000000000, 0.000000000000000000, 1.000000000000000000 ) ) ;
#4288 = VERTEX_POINT ( 'NONE', #1458 ) ;
#4289 = AXIS2_PLACEMENT_3D ( 'NONE', #10496, #8648, #6721 ) ;
#4290 = EDGE_CURVE ( 'NONE', #11388, #6435, #9925, .T. ) ;
#4291 = CARTESIAN_POINT ( 'NONE',  ( -826.4736066356965694, 82.92053275976070381, -95.16834756612315971 ) ) ;
#4292 = CARTESIAN_POINT ( 'NONE',  ( 0.000000000000000000, 0.000000000000000000, 9.000000000000000000 ) ) ;
#4293 = ORIENTED_EDGE ( 'NONE', *, *, #3087, .F. ) ;
#4294 = CARTESIAN_POINT ( 'NONE',  ( -305.0000000000000568, 81.99999999999995737, -159.6807709998038547 ) ) ;
#4295 = ORIENTED_EDGE ( 'NONE', *, *, #86, .F. ) ;
#4296 = CARTESIAN_POINT ( 'NONE',  ( -126.4213562373094959, -492.9999999999998863, 2.255140518769849223E-14 ) ) ;
#4297 = AXIS2_PLACEMENT_3D ( 'NONE', #2396, #6174, #9938 ) ;
#4298 = AXIS2_PLACEMENT_3D ( 'NONE', #10693, #2920, #5098 ) ;
#4299 = CARTESIAN_POINT ( 'NONE',  ( -1061.104375862967800, 103.3839434440458547, -103.3307627799635924 ) ) ;
#4300 = FACE_OUTER_BOUND ( 'NONE', #7491, .T. ) ;
#4301 = ORIENTED_EDGE ( 'NONE', *, *, #11364, .F. ) ;
#4302 = DIRECTION ( 'NONE',  ( -8.163404592832030268E-17, 1.000000000000000000, -0.000000000000000000 ) ) ;
#4303 = EDGE_LOOP ( 'NONE', ( #3017, #1012, #11828 ) ) ;
#4304 = PRESENTATION_LAYER_ASSIGNMENT (  '', '', ( #751 ) ) ;
#4305 = FACE_BOUND ( 'NONE', #197, .T. ) ;
#4306 = DIRECTION ( 'NONE',  ( 0.000000000000000000, 1.000000000000000000, 0.000000000000000000 ) ) ;
#4307 = VERTEX_POINT ( 'NONE', #525 ) ;
#4308 = CARTESIAN_POINT ( 'NONE',  ( -828.8285638327247398, 78.67432280806576728, -154.5823979888776591 ) ) ;
#4309 = CARTESIAN_POINT ( 'NONE',  ( -1012.527716518103489, 86.38194213450553605, -94.48732055948642028 ) ) ;
#4310 = DIRECTION ( 'NONE',  ( 1.186840563529527301E-16, -1.000000000000000000, 0.000000000000000000 ) ) ;
#4311 = CARTESIAN_POINT ( 'NONE',  ( -1024.691966601152672, 118.8493250655916142, -124.6807709998039400 ) ) ;
#4312 = MECHANICAL_DESIGN_GEOMETRIC_PRESENTATION_REPRESENTATION (  '', ( #4897 ), #11232 ) ;
#4313 = CARTESIAN_POINT ( 'NONE',  ( 6.257111856936825515E-13, 152.0000000000000000, -73.92135623730948168 ) ) ;
#4314 = CARTESIAN_POINT ( 'NONE',  ( -819.3325619471207801, 76.46264315494589425, -143.9014485902359297 ) ) ;
#4315 = FACE_BOUND ( 'NONE', #7098, .T. ) ;
#4316 = CARTESIAN_POINT ( 'NONE',  ( -379.1619848709566440, 61.99999999999992184, -124.6807709998039542 ) ) ;
#4317 = CARTESIAN_POINT ( 'NONE',  ( -823.1736050761592196, 83.64219470983154281, -95.24653602621386028 ) ) ;
#4318 = EDGE_LOOP ( 'NONE', ( #11882, #6547, #5750, #2932, #1803, #289 ) ) ;
#4319 = CYLINDRICAL_SURFACE ( 'NONE', #11022, 7.500000000000007105 ) ;
#4320 = CARTESIAN_POINT ( 'NONE',  ( -823.7180591916842332, 117.1502831467252150, -118.7903414690680535 ) ) ;
#4321 = AXIS2_PLACEMENT_3D ( 'NONE', #686, #6436, #8367 ) ;
#4322 = EDGE_CURVE ( 'NONE', #9411, #1374, #5741, .T. ) ;
#4323 = DIRECTION ( 'NONE',  ( -1.186840563529527301E-16, 1.000000000000000000, -0.000000000000000000 ) ) ;
#4324 = CARTESIAN_POINT ( 'NONE',  ( -142.5000000000000000, -9.213203435596451385, -126.4213562373084301 ) ) ;
#4325 = DIRECTION ( 'NONE',  ( 0.000000000000000000, 0.000000000000000000, 1.000000000000000000 ) ) ;
#4326 = CARTESIAN_POINT ( 'NONE',  ( 120.8820948793965186, 12.00000000000000000, -179.1989091883332890 ) ) ;
#4327 = ORIENTED_EDGE ( 'NONE', *, *, #10098, .T. ) ;
#4328 = AXIS2_PLACEMENT_3D ( 'NONE', #5366, #9142, #8234 ) ;
#4329 = ORIENTED_EDGE ( 'NONE', *, *, #7278, .T. ) ;
#4330 = CARTESIAN_POINT ( 'NONE',  ( -19.88499600238774434, 181.6747900880826592, -126.8253906927961623 ) ) ;
#4331 = CARTESIAN_POINT ( 'NONE',  ( -384.9934929388428486, 81.09111041420437971, -144.6692448832289131 ) ) ;
#4332 = CARTESIAN_POINT ( 'NONE',  ( -927.6556653798983234, 86.18751778479050074, -154.2940595301282656 ) ) ;
#4333 = CARTESIAN_POINT ( 'NONE',  ( -828.8285638327246261, 78.51036871773322900, -144.3746817049001834 ) ) ;
#4334 = FACE_OUTER_BOUND ( 'NONE', #8748, .T. ) ;
#4335 = CYLINDRICAL_SURFACE ( 'NONE', #9361, 7.499999999999992895 ) ;
#4336 = DIRECTION ( 'NONE',  ( 0.000000000000000000, 0.8660254037844375974, -0.5000000000000019984 ) ) ;
#4337 = CARTESIAN_POINT ( 'NONE',  ( -819.3359138399641779, 76.45573320715882915, -94.68090302126685742 ) ) ;
#4338 =( NAMED_UNIT ( * ) SI_UNIT ( $, .STERADIAN. ) SOLID_ANGLE_UNIT ( ) );
#4339 = AXIS2_PLACEMENT_3D ( 'NONE', #529, #11853, #9061 ) ;
#4340 = ORIENTED_EDGE ( 'NONE', *, *, #9875, .F. ) ;
#4341 = CARTESIAN_POINT ( 'NONE',  ( -1021.046747802647246, 63.38047825189622841, -146.0307792196452681 ) ) ;
#4342 = EDGE_CURVE ( 'NONE', #6027, #10270, #8850, .T. ) ;
#4343 = ORIENTED_EDGE ( 'NONE', *, *, #7747, .T. ) ;
#4344 = VERTEX_POINT ( 'NONE', #5281 ) ;
#4345 = CYLINDRICAL_SURFACE ( 'NONE', #8030, 7.500000000000012434 ) ;
#4346 = EDGE_CURVE ( 'NONE', #2139, #4019, #7474, .T. ) ;
#4347 = DIRECTION ( 'NONE',  ( -0.000000000000000000, -0.000000000000000000, -1.000000000000000000 ) ) ;
#4348 = CARTESIAN_POINT ( 'NONE',  ( -19.97760348394007579, 179.8079052437743997, -126.1102380945337558 ) ) ;
#4349 = EDGE_LOOP ( 'NONE', ( #6557, #11509, #9254, #5865 ) ) ;
#4350 = CARTESIAN_POINT ( 'NONE',  ( -142.5000000000000000, 139.9999999999999716, -126.4213562373084301 ) ) ;
#4351 = CARTESIAN_POINT ( 'NONE',  ( 2.498657532616778856E-14, -6.999999999999978684, -124.6807709998038405 ) ) ;
#4352 = ORIENTED_EDGE ( 'NONE', *, *, #10394, .T. ) ;
#4353 = EDGE_LOOP ( 'NONE', ( #3154, #11847 ) ) ;
#4354 = EDGE_CURVE ( 'NONE', #9244, #8918, #11903, .T. ) ;
#4355 = DIRECTION ( 'NONE',  ( 0.000000000000000000, 1.000000000000000000, 0.000000000000000000 ) ) ;
#4356 = EDGE_CURVE ( 'NONE', #4489, #1654, #4494, .T. ) ;
#4357 = DIRECTION ( 'NONE',  ( 0.000000000000000000, 0.000000000000000000, 1.000000000000000000 ) ) ;
#4358 = CARTESIAN_POINT ( 'NONE',  ( -927.4753839990671622, 92.66010094724835255, -94.48732055948569553 ) ) ;
#4359 = CARTESIAN_POINT ( 'NONE',  ( 28.00000000000000000, -6.000000000000000000, -27.99999999999999645 ) ) ;
#4360 = DIRECTION ( 'NONE',  ( 1.000000000000000000, 0.000000000000000000, 0.000000000000000000 ) ) ;
#4361 = ADVANCED_FACE ( 'NONE', ( #7270 ), #2566, .F. ) ;
#4362 = EDGE_CURVE ( 'NONE', #5569, #8440, #12099, .T. ) ;
#4363 = ORIENTED_EDGE ( 'NONE', *, *, #7212, .F. ) ;
#4364 = CARTESIAN_POINT ( 'NONE',  ( -20.72699427085588297, 179.8710689655571855, -123.3349751025961325 ) ) ;
#4365 = ORIENTED_EDGE ( 'NONE', *, *, #10907, .T. ) ;
#4366 = CARTESIAN_POINT ( 'NONE',  ( -826.0516380081095349, 83.16490949901579199, -154.1628641512737943 ) ) ;
#4367 = CARTESIAN_POINT ( 'NONE',  ( -1027.019426772557381, 78.04595964998433999, -95.06748246948046699 ) ) ;
#4368 = CARTESIAN_POINT ( 'NONE',  ( 0.8038475772933666441, 10.39230484541326938, -2.501782431774985704E-16 ) ) ;
#4369 = EDGE_CURVE ( 'NONE', #10481, #6037, #9056, .T. ) ;
#4370 = CARTESIAN_POINT ( 'NONE',  ( 1.874378101782966050E-12, 0.000000000000000000, 61.07864376269051121 ) ) ;
#4371 = CYLINDRICAL_SURFACE ( 'NONE', #2555, 81.99999999999998579 ) ;
#4372 = CARTESIAN_POINT ( 'NONE',  ( 20.90408460058374729, 181.4799304009739842, -122.6759650212516561 ) ) ;
#4373 = FACE_OUTER_BOUND ( 'NONE', #2372, .T. ) ;
#4374 = CARTESIAN_POINT ( 'NONE',  ( 1.249585401188644101E-12, -6.000000000000006217, 1.078643762690512986 ) ) ;
#4375 = CARTESIAN_POINT ( 'NONE',  ( -27.99999999999999645, -6.000000000000000000, -27.99999999999999645 ) ) ;
#4376 = ORIENTED_EDGE ( 'NONE', *, *, #10779, .T. ) ;
#4377 = DIRECTION ( 'NONE',  ( 0.000000000000000000, 5.522905491341382306E-16, 1.000000000000000000 ) ) ;
#4378 = CARTESIAN_POINT ( 'NONE',  ( -974.1288507787421622, 124.2142274477005657, -122.7172756069789017 ) ) ;
#4379 = CYLINDRICAL_SURFACE ( 'NONE', #839, 7.500000000000005329 ) ;
#4380 = CARTESIAN_POINT ( 'NONE',  ( 154.5043356068769071, 12.00000000000000000, -109.5666613060171670 ) ) ;
#4381 = DIRECTION ( 'NONE',  ( -1.000000000000000000, 0.000000000000000000, 0.000000000000000000 ) ) ;
#4382 = AXIS2_PLACEMENT_3D ( 'NONE', #5129, #303, #5237 ) ;
#4383 = CARTESIAN_POINT ( 'NONE',  ( 19.92456121491558463, 181.7656274153872573, -122.9373171337986008 ) ) ;
#4384 = ORIENTED_EDGE ( 'NONE', *, *, #6373, .F. ) ;
#4385 = EDGE_LOOP ( 'NONE', ( #7626, #8238, #8701, #152 ) ) ;
#4386 = CARTESIAN_POINT ( 'NONE',  ( 19.90865200055594997, 181.4799304009739842, -122.7714319726112819 ) ) ;
#4387 = DIRECTION ( 'NONE',  ( 0.000000000000000000, 0.000000000000000000, -1.000000000000000000 ) ) ;
#4388 = CARTESIAN_POINT ( 'NONE',  ( 8.937118865183856033E-16, 196.0000000000000000, -124.6807709998038405 ) ) ;
#4389 = CARTESIAN_POINT ( 'NONE',  ( -1038.028607166442953, 78.75533988487831039, -154.8742214401230797 ) ) ;
#4390 = CARTESIAN_POINT ( 'NONE',  ( -827.1548796934596339, 74.92718183615757255, -143.3900093790826418 ) ) ;
#4391 = CIRCLE ( 'NONE', #9526, 7.500000000000007105 ) ;
#4392 = CARTESIAN_POINT ( 'NONE',  ( 6.247927005943220505E-13, -6.000000000000005329, -66.42135623730949590 ) ) ;
#4393 = ORIENTED_EDGE ( 'NONE', *, *, #3501, .F. ) ;
#4394 = FACE_BOUND ( 'NONE', #11723, .T. ) ;
#4395 = SURFACE_SIDE_STYLE ('',( #10877 ) ) ;
#4396 = EDGE_LOOP ( 'NONE', ( #7406, #10772 ) ) ;
#4397 = CARTESIAN_POINT ( 'NONE',  ( -1047.844889418685170, 56.55730854968103927, -149.7857175106634315 ) ) ;
#4398 = AXIS2_PLACEMENT_3D ( 'NONE', #5701, #7558, #4036 ) ;
#4399 = EDGE_LOOP ( 'NONE', ( #12050, #5987 ) ) ;
#4400 = VERTEX_POINT ( 'NONE', #6281 ) ;
#4401 = EDGE_CURVE ( 'NONE', #4868, #10168, #11965, .T. ) ;
#4402 = CARTESIAN_POINT ( 'NONE',  ( -19.97689317482322480, 180.4398926601855067, -126.1441920888607058 ) ) ;
#4403 = DIRECTION ( 'NONE',  ( 0.000000000000000000, 1.000000000000000000, 0.000000000000000000 ) ) ;
#4404 = FACE_BOUND ( 'NONE', #3983, .T. ) ;
#4405 = EDGE_CURVE ( 'NONE', #6480, #11420, #10034, .T. ) ;
#4406 = CIRCLE ( 'NONE', #11318, 7.500000000000007105 ) ;
#4407 = EDGE_LOOP ( 'NONE', ( #1384, #4159, #415, #2025 ) ) ;
#4408 = CARTESIAN_POINT ( 'NONE',  ( -379.1617638233734624, 61.99874095070342150, -123.3668595883440986 ) ) ;
#4409 = DIRECTION ( 'NONE',  ( -8.163404592832030268E-17, 1.000000000000000000, -0.000000000000000000 ) ) ;
#4410 = ORIENTED_EDGE ( 'NONE', *, *, #389, .T. ) ;
#4411 = ORIENTED_EDGE ( 'NONE', *, *, #7892, .T. ) ;
#4412 = VECTOR ( 'NONE', #111, 1000.000000000000000 ) ;
#4413 = ADVANCED_FACE ( 'NONE', ( #5343 ), #2764, .T. ) ;
#4414 = DIRECTION ( 'NONE',  ( 0.000000000000000000, -1.000000000000000000, 0.000000000000000000 ) ) ;
#4415 = CARTESIAN_POINT ( 'NONE',  ( 20.94276857858305618, 181.6519786105751848, -124.4341959704801610 ) ) ;
#4416 = VECTOR ( 'NONE', #46, 1000.000000000000000 ) ;
#4417 = FACE_OUTER_BOUND ( 'NONE', #6757, .T. ) ;
#4418 = CARTESIAN_POINT ( 'NONE',  ( -1024.256845364730452, 79.46673622094698430, -95.06748246948041015 ) ) ;
#4419 = FACE_OUTER_BOUND ( 'NONE', #11619, .T. ) ;
#4420 = DIRECTION ( 'NONE',  ( -8.163404592832031500E-17, 1.000000000000000000, 0.000000000000000000 ) ) ;
#4421 = EDGE_LOOP ( 'NONE', ( #5251, #7757, #2175, #1265 ) ) ;
#4422 = AXIS2_PLACEMENT_3D ( 'NONE', #3723, #762, #8444 ) ;
#4423 = DIRECTION ( 'NONE',  ( -8.163404592832031500E-17, 1.000000000000000000, 0.000000000000000000 ) ) ;
#4424 = ADVANCED_FACE ( 'NONE', ( #1711, #1643 ), #718, .F. ) ;
#4425 = CIRCLE ( 'NONE', #10540, 44.00000000000000711 ) ;
#4426 = DIRECTION ( 'NONE',  ( 0.000000000000000000, 0.000000000000000000, 1.000000000000000000 ) ) ;
#4427 = DIRECTION ( 'NONE',  ( 0.000000000000000000, -0.000000000000000000, -1.000000000000000000 ) ) ;
#4428 = ORIENTED_EDGE ( 'NONE', *, *, #5184, .T. ) ;
#4429 = CARTESIAN_POINT ( 'NONE',  ( -824.4878712493014064, 83.64140073480777460, -154.1055574741608325 ) ) ;
#4430 = CARTESIAN_POINT ( 'NONE',  ( -1024.641217300039216, 73.20632742167531148, -96.78565065507991960 ) ) ;
#4431 = DIRECTION ( 'NONE',  ( -1.000000000000000000, 0.000000000000000000, 0.000000000000000000 ) ) ;
#4432 = DIRECTION ( 'NONE',  ( 1.000000000000000000, 0.000000000000000000, 0.000000000000000000 ) ) ;
#4433 = VECTOR ( 'NONE', #8622, 1000.000000000000000 ) ;
#4434 = DIRECTION ( 'NONE',  ( -0.000000000000000000, 1.000000000000000000, 7.930164461608263644E-17 ) ) ;
#4435 = CARTESIAN_POINT ( 'NONE',  ( -19.87230422438681288, 180.2683866676943296, -122.4243209296576680 ) ) ;
#4436 = CARTESIAN_POINT ( 'NONE',  ( -824.4897464405646588, 73.71539350114024103, -142.8842219741773931 ) ) ;
#4437 = CARTESIAN_POINT ( 'NONE',  ( -126.4213562373094959, -494.9999999999998863, -7.499999999999990230 ) ) ;
#4438 = CARTESIAN_POINT ( 'NONE',  ( -305.0000000000000568, 24.00000000000000711, -89.68077099980384048 ) ) ;
#4439 = EDGE_CURVE ( 'NONE', #931, #5557, #6469, .T. ) ;
#4440 = CARTESIAN_POINT ( 'NONE',  ( -823.5047064235034213, 114.4566975831562274, -136.2353035311979284 ) ) ;
#4441 = EDGE_LOOP ( 'NONE', ( #6502, #4537 ) ) ;
#4442 = LINE ( 'NONE', #11916, #5050 ) ;
#4443 = CARTESIAN_POINT ( 'NONE',  ( -904.1919162299243453, 124.8346192645297918, -118.7903414690678119 ) ) ;
#4444 = AXIS2_PLACEMENT_3D ( 'NONE', #4479, #4671, #4611 ) ;
#4445 = VECTOR ( 'NONE', #2316, 1000.000000000000000 ) ;
#4446 = FACE_OUTER_BOUND ( 'NONE', #5422, .T. ) ;
#4447 = DIRECTION ( 'NONE',  ( -0.000000000000000000, 1.000000000000000000, 7.930164461608263644E-17 ) ) ;
#4448 = CARTESIAN_POINT ( 'NONE',  ( -372.1690766668580750, 62.27098734669634439, -104.8338495486176640 ) ) ;
#4449 = CARTESIAN_POINT ( 'NONE',  ( 21.01102415922771982, 181.7037659814379538, -124.9847730909611130 ) ) ;
#4450 = ORIENTED_EDGE ( 'NONE', *, *, #6817, .T. ) ;
#4451 = ORIENTED_EDGE ( 'NONE', *, *, #6855, .T. ) ;
#4452 = CARTESIAN_POINT ( 'NONE',  ( -19.86218813316839160, 179.0832429894416862, -127.0274896556490631 ) ) ;
#4453 = DIRECTION ( 'NONE',  ( -0.000000000000000000, -0.000000000000000000, -1.000000000000000000 ) ) ;
#4454 = CARTESIAN_POINT ( 'NONE',  ( -1037.899050076299318, 86.18944477603574228, -154.2940595301282656 ) ) ;
#4455 = CARTESIAN_POINT ( 'NONE',  ( -370.4401466759219375, 106.8513018378076822, -134.3428354745942102 ) ) ;
#4456 = CARTESIAN_POINT ( 'NONE',  ( 144.0488662551573782, 12.00000000000000000, -154.4077238332702393 ) ) ;
#4457 = CARTESIAN_POINT ( 'NONE',  ( -1011.935294340112478, 99.50314415908300703, -152.5758913445291967 ) ) ;
#4458 = CARTESIAN_POINT ( 'NONE',  ( -87.04832655144203102, 12.00000000000000000, -225.4289243767377116 ) ) ;
#4459 = ORIENTED_EDGE ( 'NONE', *, *, #1495, .F. ) ;
#4460 = CARTESIAN_POINT ( 'NONE',  ( -818.8609195637731091, 78.01770880634862237, -94.71076406233586908 ) ) ;
#4461 = EDGE_CURVE ( 'NONE', #4719, #1969, #3542, .T. ) ;
#4462 = DIRECTION ( 'NONE',  ( -0.000000000000000000, 1.000000000000000000, 7.930164461608263644E-17 ) ) ;
#4463 = VERTEX_POINT ( 'NONE', #7334 ) ;
#4464 = CARTESIAN_POINT ( 'NONE',  ( -126.4213562373094959, 0.000000000000000000, -7.499999999999990230 ) ) ;
#4465 = CARTESIAN_POINT ( 'NONE',  ( -1062.301584968959560, 67.66927912025090563, -152.5758913445295377 ) ) ;
#4466 = CIRCLE ( 'NONE', #11368, 7.500000000000007105 ) ;
#4467 = CARTESIAN_POINT ( 'NONE',  ( -20.71964524312745937, 180.2041921146310415, -123.3053720114591272 ) ) ;
#4468 = ORIENTED_EDGE ( 'NONE', *, *, #9777, .F. ) ;
#4469 = ORIENTED_EDGE ( 'NONE', *, *, #9412, .F. ) ;
#4470 = CARTESIAN_POINT ( 'NONE',  ( -21.06761139726929244, 181.2453226294160515, -126.0007492840280179 ) ) ;
#4471 = VERTEX_POINT ( 'NONE', #11102 ) ;
#4472 = CARTESIAN_POINT ( 'NONE',  ( -372.6372986097472904, 62.76969066101212746, -130.2274012109807302 ) ) ;
#4473 = DIRECTION ( 'NONE',  ( 1.000000000000000000, 0.000000000000000000, 0.000000000000000000 ) ) ;
#4474 = VERTEX_POINT ( 'NONE', #12167 ) ;
#4475 = CIRCLE ( 'NONE', #11381, 7.500000000000012434 ) ;
#4476 = VERTEX_POINT ( 'NONE', #6404 ) ;
#4477 = CARTESIAN_POINT ( 'NONE',  ( -1038.708781889657075, 41.03774456592552156, -130.5712005305402670 ) ) ;
#4478 = EDGE_CURVE ( 'NONE', #1936, #2170, #5471, .T. ) ;
#4479 = CARTESIAN_POINT ( 'NONE',  ( -59.99999999999998579, -9.213203435596451385, -126.4213562373090696 ) ) ;
#4480 = EDGE_CURVE ( 'NONE', #4637, #5145, #3717, .T. ) ;
#4481 = CARTESIAN_POINT ( 'NONE',  ( 0.01885174614965850343, 0.8831628876357843216, 8.999999999999998224 ) ) ;
#4482 = DIRECTION ( 'NONE',  ( -6.195440985631455317E-17, 0.000000000000000000, 1.000000000000000000 ) ) ;
#4483 = LINE ( 'NONE', #8257, #3293 ) ;
#4484 = AXIS2_PLACEMENT_3D ( 'NONE', #1631, #10345, #10285 ) ;
#4485 = CARTESIAN_POINT ( 'NONE',  ( -975.3893330992572146, 71.12659035875115876, -95.06748246948035330 ) ) ;
#4486 = CARTESIAN_POINT ( 'NONE',  ( 1.874378101782966050E-12, 12.00000000000000000, 53.57864376269050410 ) ) ;
#4487 = CARTESIAN_POINT ( 'NONE',  ( 57.50000000000000000, 6.167321280506070407E-16, -5.035999999999999588 ) ) ;
#4488 = SHAPE_REPRESENTATION ( 'Bending Angle Gauge Plate', ( #11957 ), #6826 ) ;
#4489 = VERTEX_POINT ( 'NONE', #9495 ) ;
#4490 = DIRECTION ( 'NONE',  ( -1.000000000000000000, 0.000000000000000000, 0.000000000000000000 ) ) ;
#4491 = ORIENTED_EDGE ( 'NONE', *, *, #6929, .T. ) ;
#4492 = CARTESIAN_POINT ( 'NONE',  ( -1023.860074334734577, 85.97273905232950142, -94.48732055948609343 ) ) ;
#4493 = CIRCLE ( 'NONE', #7846, 7.500000000000012434 ) ;
#4494 = LINE ( 'NONE', #3609, #10624 ) ;
#4495 = DIRECTION ( 'NONE',  ( -0.1216852752136955151, 0.3205457103956290688, 0.9393844481058480911 ) ) ;
#4496 = EDGE_CURVE ( 'NONE', #12134, #3288, #92, .T. ) ;
#4497 = DIRECTION ( 'NONE',  ( 0.000000000000000000, 0.000000000000000000, 1.000000000000000000 ) ) ;
#4498 = DIRECTION ( 'NONE',  ( 0.000000000000000000, -1.000000000000000000, -2.312964634635740689E-15 ) ) ;
#4499 = CARTESIAN_POINT ( 'NONE',  ( -19.96087997506392142, 179.9125189710396739, -123.2164587046221271 ) ) ;
#4500 = LINE ( 'NONE', #9253, #5201 ) ;
#4501 = AXIS2_PLACEMENT_3D ( 'NONE', #3215, #4892, #5819 ) ;
#4502 = ADVANCED_FACE ( 'NONE', ( #10420 ), #2336, .T. ) ;
#4503 = ORIENTED_EDGE ( 'NONE', *, *, #8108, .F. ) ;
#4504 = CARTESIAN_POINT ( 'NONE',  ( -370.6529647798200813, 57.71370879208589599, -136.1226710876236439 ) ) ;
#4505 = FACE_OUTER_BOUND ( 'NONE', #3838, .T. ) ;
#4506 = ORIENTED_EDGE ( 'NONE', *, *, #4439, .F. ) ;
#4507 = CARTESIAN_POINT ( 'NONE',  ( -1024.722591077092829, 118.3980260646366958, -118.7903414690678403 ) ) ;
#4508 = FACE_OUTER_BOUND ( 'NONE', #5762, .T. ) ;
#4509 = CARTESIAN_POINT ( 'NONE',  ( 3.123963502971610252E-13, -6.000000000000005329, -96.42135623730949590 ) ) ;
#4510 = CARTESIAN_POINT ( 'NONE',  ( 151.3258811035896656, 0.000000000000000000, -56.13263083939798292 ) ) ;
#4511 = CIRCLE ( 'NONE', #10235, 8.999999999999998224 ) ;
#4512 = EDGE_CURVE ( 'NONE', #882, #10332, #3869, .T. ) ;
#4513 = CARTESIAN_POINT ( 'NONE',  ( 19.99920057787401717, 181.7064984983803129, -124.8736205325594284 ) ) ;
#4514 = EDGE_CURVE ( 'NONE', #7319, #1192, #1900, .T. ) ;
#4515 = VERTEX_POINT ( 'NONE', #920 ) ;
#4516 = EDGE_CURVE ( 'NONE', #7116, #90, #11536, .T. ) ;
#4517 = VERTEX_POINT ( 'NONE', #5601 ) ;
#4518 = AXIS2_PLACEMENT_3D ( 'NONE', #11410, #6710, #3006 ) ;
#4519 = DIRECTION ( 'NONE',  ( 0.000000000000000000, 1.000000000000000000, 0.000000000000000000 ) ) ;
#4520 = DIRECTION ( 'NONE',  ( 0.000000000000000000, 1.000000000000000000, 0.000000000000000000 ) ) ;
#4521 = CARTESIAN_POINT ( 'NONE',  ( -1012.226803665787770, 93.06815595962714838, -154.2940595301283224 ) ) ;
#4522 = CARTESIAN_POINT ( 'NONE',  ( -372.4515014085467897, 101.8909246911471200, -126.9092234254810876 ) ) ;
#4523 = VECTOR ( 'NONE', #6722, 1000.000000000000000 ) ;
#4524 = CARTESIAN_POINT ( 'NONE',  ( 0.3563104543936356228, 9.539178283403849434, -1.477658550686871353 ) ) ;
#4525 = CARTESIAN_POINT ( 'NONE',  ( -187.5000000000000000, 139.9999999999999716, -126.4213562373082453 ) ) ;
#4526 = CARTESIAN_POINT ( 'NONE',  ( -927.2951026182241776, 99.13268410970675859, -154.2940595301278961 ) ) ;
#4527 = CARTESIAN_POINT ( 'NONE',  ( 20.77152989773913916, 180.9696350864299461, -123.5256872951201643 ) ) ;
#4528 = ORIENTED_EDGE ( 'NONE', *, *, #6284, .T. ) ;
#4529 = LINE ( 'NONE', #6367, #1955 ) ;
#4530 = CARTESIAN_POINT ( 'NONE',  ( -180.0000000000000000, 24.00000000000001421, -126.4213562373082453 ) ) ;
#4531 = ORIENTED_EDGE ( 'NONE', *, *, #2299, .T. ) ;
#4532 = CARTESIAN_POINT ( 'NONE',  ( -120.8820948793972434, 12.00000000000000000, -194.1989091883324363 ) ) ;
#4533 = CARTESIAN_POINT ( 'NONE',  ( -1038.158164256572263, 71.32123499372137587, -154.2940595301283224 ) ) ;
#4534 = CONICAL_SURFACE ( 'NONE', #775, 9.000000000000000000, 1.047197551196600296 ) ;
#4535 = CARTESIAN_POINT ( 'NONE',  ( 19.87268743161337170, 178.9255784920988503, -126.9338343023757290 ) ) ;
#4536 = ORIENTED_EDGE ( 'NONE', *, *, #9981, .T. ) ;
#4537 = ORIENTED_EDGE ( 'NONE', *, *, #6350, .F. ) ;
#4538 = CARTESIAN_POINT ( 'NONE',  ( -19.83253561012729449, 179.9725903414323795, -127.2636293852243483 ) ) ;
#4539 = LINE ( 'NONE', #1557, #532 ) ;
#4540 = ORIENTED_EDGE ( 'NONE', *, *, #5688, .F. ) ;
#4541 = CARTESIAN_POINT ( 'NONE',  ( -126.4213562373094959, 12.00000000000000000, 2.255140518769849223E-14 ) ) ;
#4542 = CARTESIAN_POINT ( 'NONE',  ( -373.8419305655268090, 67.98320497006626795, -139.0453867504895129 ) ) ;
#4543 = CARTESIAN_POINT ( 'NONE',  ( 7.653191805780027529E-16, 138.9999999999999716, -126.4213562373094959 ) ) ;
#4544 = CLOSED_SHELL ( 'NONE', ( #4609, #3807, #12155, #11684, #8450, #1388, #10453, #8041 ) ) ;
#4545 = CARTESIAN_POINT ( 'NONE',  ( 2.186774452080127126E-12, 0.000000000000000000, 83.57864376269050410 ) ) ;
#4546 = DIRECTION ( 'NONE',  ( 1.000000000000000000, 0.000000000000000000, -0.000000000000000000 ) ) ;
#4547 = CARTESIAN_POINT ( 'NONE',  ( 21.06147608529250803, 178.9413095352420271, -125.7232933582278491 ) ) ;
#4548 = CARTESIAN_POINT ( 'NONE',  ( -1038.028607166439997, 78.75533988487829617, -94.48732055948607922 ) ) ;
#4549 = DIRECTION ( 'NONE',  ( 0.000000000000000000, 1.000000000000000000, 0.000000000000000000 ) ) ;
#4550 = CARTESIAN_POINT ( 'NONE',  ( 6.257111856936825515E-13, 164.0000000000000000, -73.92135623730948168 ) ) ;
#4551 = CARTESIAN_POINT ( 'NONE',  ( 30.00000000000000000, -492.9999999999998863, -30.00000000000000000 ) ) ;
#4552 = CARTESIAN_POINT ( 'NONE',  ( -954.5692209181572707, 49.02792041507773746, -126.6442663926294045 ) ) ;
#4553 = VERTEX_POINT ( 'NONE', #4800 ) ;
#4554 = FACE_BOUND ( 'NONE', #8597, .T. ) ;
#4555 = SURFACE_STYLE_USAGE ( .BOTH. , #3800 ) ;
#4556 = ORIENTED_EDGE ( 'NONE', *, *, #10469, .T. ) ;
#4557 = CARTESIAN_POINT ( 'NONE',  ( 144.0488662551573782, 12.00000000000000000, -146.9077238332702109 ) ) ;
#4558 = CARTESIAN_POINT ( 'NONE',  ( -1020.755281158177013, 68.40999151392674094, -99.57582448894541471 ) ) ;
#4559 = CARTESIAN_POINT ( 'NONE',  ( 0.09252763182291869060, 8.674330214978045461, 2.975619346028167911 ) ) ;
#4560 = LINE ( 'NONE', #3748, #9735 ) ;
#4561 = DIRECTION ( 'NONE',  ( -0.000000000000000000, 1.000000000000000000, -0.000000000000000000 ) ) ;
#4562 = CARTESIAN_POINT ( 'NONE',  ( -821.5852935318491745, 74.19369191907351535, -106.2666214282630790 ) ) ;
#4563 = CARTESIAN_POINT ( 'NONE',  ( -19.95977122504825729, 180.0239105065436434, -123.1990849849620844 ) ) ;
#4564 = DIRECTION ( 'NONE',  ( -1.000000000000000000, -1.186840563529527301E-16, 0.000000000000000000 ) ) ;
#4565 = EDGE_CURVE ( 'NONE', #11519, #3632, #9614, .T. ) ;
#4566 = ORIENTED_EDGE ( 'NONE', *, *, #6321, .T. ) ;
#4567 = ORIENTED_EDGE ( 'NONE', *, *, #6967, .F. ) ;
#4568 = CARTESIAN_POINT ( 'NONE',  ( -370.4431240880636551, 57.15653990293812825, -114.9924028573050663 ) ) ;
#4569 = CARTESIAN_POINT ( 'NONE',  ( -382.1463966336086173, 96.15313453893932660, -110.4906001672614622 ) ) ;
#4570 = EDGE_CURVE ( 'NONE', #3156, #1708, #357, .T. ) ;
#4571 = ORIENTED_EDGE ( 'NONE', *, *, #10375, .T. ) ;
#4572 = DIRECTION ( 'NONE',  ( -1.186840563529527301E-16, 1.000000000000000000, 0.000000000000000000 ) ) ;
#4573 = B_SPLINE_CURVE_WITH_KNOTS ( 'NONE', 3,
 ( #5430, #745, #4524, #8301, #3568, #2472 ),
 .UNSPECIFIED., .F., .F.,
 ( 4, 2, 4 ),
 ( 2.380730968232385423E-07, 0.002629065763328362199, 0.005257893453559901037 ),
 .UNSPECIFIED. ) ;
#4574 = CARTESIAN_POINT ( 'NONE',  ( -823.7697810748813936, 117.7733807739867871, -122.7172756069790438 ) ) ;
#4575 = AXIS2_PLACEMENT_3D ( 'NONE', #4917, #215, #4064 ) ;
#4576 = CARTESIAN_POINT ( 'NONE',  ( -141.4213562373095101, -494.9999999999998863, 3.644282033693712520E-14 ) ) ;
#4577 = DIRECTION ( 'NONE',  ( 0.000000000000000000, 0.000000000000000000, 1.000000000000000000 ) ) ;
#4578 = CYLINDRICAL_SURFACE ( 'NONE', #6419, 7.500000000000007105 ) ;
#4579 = ADVANCED_FACE ( 'NONE', ( #7519 ), #5663, .F. ) ;
#4580 = CARTESIAN_POINT ( 'NONE',  ( 19.97971902011833123, 180.8960314115462040, -126.0058985864737053 ) ) ;
#4581 = VERTEX_POINT ( 'NONE', #1160 ) ;
#4582 = EDGE_LOOP ( 'NONE', ( #1503, #3966 ) ) ;
#4583 = DIRECTION ( 'NONE',  ( -1.000000000000000000, -0.000000000000000000, -0.000000000000000000 ) ) ;
#4584 = DIRECTION ( 'NONE',  ( -1.224646799147353207E-16, -3.748982739283705415E-33, 1.000000000000000000 ) ) ;
#4585 = CARTESIAN_POINT ( 'NONE',  ( -1023.463303304735746, 92.47874188371233117, -154.2940595301281519 ) ) ;
#4586 = CARTESIAN_POINT ( 'NONE',  ( 9.371890508914830252E-13, 164.0000000000000000, -36.42135623730948168 ) ) ;
#4587 = SURFACE_SIDE_STYLE ('',( #815 ) ) ;
#4588 = DIRECTION ( 'NONE',  ( 3.061276722312011504E-17, -1.000000000000000000, 0.000000000000000000 ) ) ;
#4589 = DIRECTION ( 'NONE',  ( -8.163404592832030268E-17, 1.000000000000000000, -0.000000000000000000 ) ) ;
#4590 = ORIENTED_EDGE ( 'NONE', *, *, #3885, .F. ) ;
#4591 = CARTESIAN_POINT ( 'NONE',  ( 6.247927005943220505E-13, -6.000000000000005329, -66.42135623730949590 ) ) ;
#4592 = CYLINDRICAL_SURFACE ( 'NONE', #9651, 7.500000000000007105 ) ;
#4593 = AXIS2_PLACEMENT_3D ( 'NONE', #10809, #8718, #7039 ) ;
#4594 = EDGE_CURVE ( 'NONE', #3971, #7586, #9377, .T. ) ;
#4595 = ORIENTED_EDGE ( 'NONE', *, *, #4461, .T. ) ;
#4596 = CARTESIAN_POINT ( 'NONE',  ( -819.8389179520123662, 63.91331975908080665, -154.2940595301278677 ) ) ;
#4597 = CARTESIAN_POINT ( 'NONE',  ( 19.97025581332069422, 182.5233676713443174, -125.7761851878406105 ) ) ;
#4598 = EDGE_LOOP ( 'NONE', ( #5883, #3341 ) ) ;
#4599 = ADVANCED_FACE ( 'NONE', ( #4746 ), #4912, .F. ) ;
#4600 = AXIS2_PLACEMENT_3D ( 'NONE', #4735, #10407, #11523 ) ;
#4601 = VERTEX_POINT ( 'NONE', #7641 ) ;
#4602 = VECTOR ( 'NONE', #6982, 1000.000000000000000 ) ;
#4603 = CARTESIAN_POINT ( 'NONE',  ( -19.98958826779223230, 181.4702305597406848, -125.4918071840122735 ) ) ;
#4604 = CARTESIAN_POINT ( 'NONE',  ( -828.5728621739538085, 77.06309091183307203, -105.2972035265141528 ) ) ;
#4605 = VERTEX_POINT ( 'NONE', #3804 ) ;
#4606 = CARTESIAN_POINT ( 'NONE',  ( -372.9391702816300835, 63.88999388380243261, -133.3467129973068666 ) ) ;
#4607 = DIRECTION ( 'NONE',  ( -1.000000000000000000, 0.000000000000000000, 0.000000000000000000 ) ) ;
#4609 = ADVANCED_FACE ( 'NONE', ( #7576 ), #9837, .T. ) ;
#4608 = FACE_OUTER_BOUND ( 'NONE', #5824, .T. ) ;
#4610 = VECTOR ( 'NONE', #1382, 1000.000000000000000 ) ;
#4611 = DIRECTION ( 'NONE',  ( -1.000000000000000000, 0.000000000000000000, 0.000000000000000000 ) ) ;
#4612 = CARTESIAN_POINT ( 'NONE',  ( 0.09252763182291165456, -6.914127053141829293, 6.024380653971844524 ) ) ;
#4613 = LINE ( 'NONE', #9482, #11534 ) ;
#4614 = CARTESIAN_POINT ( 'NONE',  ( -1012.527716518103489, 86.38194213450553605, -94.48732055948642028 ) ) ;
#4615 = DIRECTION ( 'NONE',  ( -1.000000000000000000, 0.000000000000000000, 0.000000000000000000 ) ) ;
#4616 = DIRECTION ( 'NONE',  ( -1.000000000000000000, 0.000000000000000000, 0.000000000000000000 ) ) ;
#4617 = ORIENTED_EDGE ( 'NONE', *, *, #3077, .F. ) ;
#4618 = CARTESIAN_POINT ( 'NONE',  ( -820.0597211274471192, 81.97619047958252736, -144.6820902952096901 ) ) ;
#4619 = DIRECTION ( 'NONE',  ( 0.000000000000000000, -1.000000000000000000, 0.000000000000000000 ) ) ;
#4620 = CARTESIAN_POINT ( 'NONE',  ( -372.4687937583217945, 100.6702782477001819, -103.5591500974845047 ) ) ;
#4621 = VERTEX_POINT ( 'NONE', #6651 ) ;
#4622 = ADVANCED_FACE ( 'NONE', ( #10483 ), #4852, .F. ) ;
#4623 = CARTESIAN_POINT ( 'NONE',  ( -1025.000791045973756, 67.42844482392702332, -99.57582448894532945 ) ) ;
#4624 = CIRCLE ( 'NONE', #11521, 7.500000000000007105 ) ;
#4625 = CARTESIAN_POINT ( 'NONE',  ( -6.499999999999979572, -6.999999999999979572, -124.6807709998038405 ) ) ;
#4626 = CARTESIAN_POINT ( 'NONE',  ( -823.8285638327247398, 78.67432280806536937, -158.6807709998041673 ) ) ;
#4627 = DIRECTION ( 'NONE',  ( 0.000000000000000000, 1.000000000000000000, 0.000000000000000000 ) ) ;
#4628 = DIRECTION ( 'NONE',  ( -0.7071067811865477948, 0.000000000000000000, -0.7071067811865473507 ) ) ;
#4629 = CARTESIAN_POINT ( 'NONE',  ( -820.0492617104155215, 75.38478674231490118, -105.8049000242699833 ) ) ;
#4630 = CARTESIAN_POINT ( 'NONE',  ( -19.87341384624713569, 180.4358019248037692, -122.4339773266618323 ) ) ;
#4631 = CARTESIAN_POINT ( 'NONE',  ( 14.74749198504306591, 180.2041921146325762, -184.6327933705057376 ) ) ;
#4632 = CIRCLE ( 'NONE', #10729, 1.499999999999999112 ) ;
#4633 = CIRCLE ( 'NONE', #11922, 7.500000000000007105 ) ;
#4634 = EDGE_LOOP ( 'NONE', ( #1677, #9137, #10456, #8973 ) ) ;
#4635 = CARTESIAN_POINT ( 'NONE',  ( -371.3925255517432333, 59.81623701251285752, -140.7297140340658927 ) ) ;
#4636 = CARTESIAN_POINT ( 'NONE',  ( -374.8878514016580539, 86.86219835938075562, -105.2522987037355477 ) ) ;
#4637 = VERTEX_POINT ( 'NONE', #7702 ) ;
#4638 = CARTESIAN_POINT ( 'NONE',  ( -1014.170783943992433, 114.7803637426472534, -107.9061927053325292 ) ) ;
#4639 = CARTESIAN_POINT ( 'NONE',  ( 2.187692937179487324E-12, -6.000000000000004441, 76.07864376269048989 ) ) ;
#4640 = CIRCLE ( 'NONE', #5607, 7.500000000000013323 ) ;
#4641 = ADVANCED_FACE ( 'NONE', ( #6766 ), #8697, .F. ) ;
#4642 = AXIS2_PLACEMENT_3D ( 'NONE', #3414, #6154, #8075 ) ;
#4643 = AXIS2_PLACEMENT_3D ( 'NONE', #6767, #6893, #11538 ) ;
#4644 = CARTESIAN_POINT ( 'NONE',  ( 19.99652087076804818, 181.6001326330613779, -124.1032781992507523 ) ) ;
#4645 = EDGE_CURVE ( 'NONE', #1342, #2015, #6742, .T. ) ;
#4646 = ORIENTED_EDGE ( 'NONE', *, *, #724, .T. ) ;
#4647 = DIRECTION ( 'NONE',  ( -0.000000000000000000, -1.000000000000000000, -0.000000000000000000 ) ) ;
#4648 = DIRECTION ( 'NONE',  ( -1.000000000000000000, -0.000000000000000000, -0.000000000000000000 ) ) ;
#4649 = CARTESIAN_POINT ( 'NONE',  ( -1011.662592067699165, 105.4443429699074244, -149.7857175106632326 ) ) ;
#4650 = AXIS2_PLACEMENT_3D ( 'NONE', #8607, #8546, #6628 ) ;
#4651 =( LENGTH_UNIT ( ) NAMED_UNIT ( * ) SI_UNIT ( .MILLI., .METRE. ) );
#4652 = DIRECTION ( 'NONE',  ( -1.000000000000000000, 0.000000000000000000, 0.000000000000000000 ) ) ;
#4653 = VECTOR ( 'NONE', #5823, 1000.000000000000000 ) ;
#4654 = DIRECTION ( 'NONE',  ( 0.000000000000000000, 1.000000000000000000, 0.000000000000000000 ) ) ;
#4655 = VERTEX_POINT ( 'NONE', #7945 ) ;
#4656 = DIRECTION ( 'NONE',  ( 0.000000000000000000, 0.000000000000000000, 1.000000000000000000 ) ) ;
#4657 = ORIENTED_EDGE ( 'NONE', *, *, #11211, .T. ) ;
#4658 = CARTESIAN_POINT ( 'NONE',  ( -955.6263874535649165, 86.32439835342530898, -154.8742214401227670 ) ) ;
#4659 = CARTESIAN_POINT ( 'NONE',  ( 4.255174644013695128E-15, 25.00000000000002132, -126.4213562373094959 ) ) ;
#4660 = EDGE_LOOP ( 'NONE', ( #1170, #8764, #5140, #10036 ) ) ;
#4661 = CIRCLE ( 'NONE', #8418, 8.999999999999998224 ) ;
#4662 = ORIENTED_EDGE ( 'NONE', *, *, #580, .F. ) ;
#4663 = EDGE_CURVE ( 'NONE', #6035, #4517, #9888, .T. ) ;
#4664 = CARTESIAN_POINT ( 'NONE',  ( 6.899999999999999467, 5.196152422706624030, -9.000000000000000000 ) ) ;
#4665 = CARTESIAN_POINT ( 'NONE',  ( -21.05626678059735823, 181.5387050158279010, -125.5955412462414813 ) ) ;
#4666 = EDGE_LOOP ( 'NONE', ( #3714, #7552, #1376, #2606 ) ) ;
#4667 = CARTESIAN_POINT ( 'NONE',  ( -371.5191645905044879, 60.19565412010540939, -141.4135686812714141 ) ) ;
#4668 = DIRECTION ( 'NONE',  ( -0.000000000000000000, 1.000000000000000000, 0.000000000000000000 ) ) ;
#4669 = CARTESIAN_POINT ( 'NONE',  ( -180.0000000000000000, -9.213203435596478030, -126.4213562373082453 ) ) ;
#4670 =( GEOMETRIC_REPRESENTATION_CONTEXT ( 3 ) GLOBAL_UNCERTAINTY_ASSIGNED_CONTEXT ( ( #4916 ) ) GLOBAL_UNIT_ASSIGNED_CONTEXT ( ( #3090, #4938, #11564 ) ) REPRESENTATION_CONTEXT ( 'NONE', 'WORKASPACE' ) );
#4671 = DIRECTION ( 'NONE',  ( -8.163404592832030268E-17, 1.000000000000000000, -0.000000000000000000 ) ) ;
#4672 = EDGE_CURVE ( 'NONE', #9067, #10332, #7843, .T. ) ;
#4673 = PLANE ( 'NONE',  #5457 ) ;
#4674 = CARTESIAN_POINT ( 'NONE',  ( -305.0000000000000568, 81.99999999999995737, -159.6807709998038547 ) ) ;
#4675 = EDGE_CURVE ( 'NONE', #6037, #5102, #6544, .T. ) ;
#4676 = CARTESIAN_POINT ( 'NONE',  ( -1025.000791045973756, 67.42844482392702332, -99.57582448894532945 ) ) ;
#4677 = DIRECTION ( 'NONE',  ( 0.000000000000000000, 0.000000000000000000, 1.000000000000000000 ) ) ;
#4678 = CARTESIAN_POINT ( 'NONE',  ( -998.0431609429218724, 37.14019503514174403, -126.6442663926292340 ) ) ;
#4679 = AXIS2_PLACEMENT_3D ( 'NONE', #3496, #11051, #8806 ) ;
#4680 = CARTESIAN_POINT ( 'NONE',  ( -823.5011194091157449, 83.67446401253090471, -144.6105519893422127 ) ) ;
#4681 = CARTESIAN_POINT ( 'NONE',  ( -954.1708249681001917, 122.1961423320944249, -136.2353035311976157 ) ) ;
#4682 = ORIENTED_EDGE ( 'NONE', *, *, #14, .T. ) ;
#4683 = CARTESIAN_POINT ( 'NONE',  ( -822.5351658412957931, 83.51517767605524512, -144.6233963009597687 ) ) ;
#4684 = DIRECTION ( 'NONE',  ( 0.000000000000000000, 0.000000000000000000, 1.000000000000000000 ) ) ;
#4685 = PRESENTATION_STYLE_ASSIGNMENT (( #4555 ) ) ;
#4686 = ORIENTED_EDGE ( 'NONE', *, *, #307, .F. ) ;
#4687 = DIRECTION ( 'NONE',  ( 1.000000000000000000, 0.000000000000000000, 0.000000000000000000 ) ) ;
#4688 = CARTESIAN_POINT ( 'NONE',  ( -1032.391769651399727, 55.42093464310126905, -103.3307627799637487 ) ) ;
#4689 = DIRECTION ( 'NONE',  ( 0.000000000000000000, 0.000000000000000000, 1.000000000000000000 ) ) ;
#4690 = CARTESIAN_POINT ( 'NONE',  ( 20.77152989773913916, 180.9696350864299461, -123.5256872951201643 ) ) ;
#4691 = DIRECTION ( 'NONE',  ( 0.000000000000000000, 1.000000000000000000, -0.000000000000000000 ) ) ;
#4692 = AXIS2_PLACEMENT_3D ( 'NONE', #2556, #7259, #7506 ) ;
#4693 = UNCERTAINTY_MEASURE_WITH_UNIT (LENGTH_MEASURE( 1.000000000000000082E-05 ), #8076, 'distance_accuracy_value', 'NONE');
#4694 = CARTESIAN_POINT ( 'NONE',  ( -852.9318753287178652, 113.3383058689773151, -107.9061927053323302 ) ) ;
#4695 = CARTESIAN_POINT ( 'NONE',  ( -828.6675604493455012, 77.37337224769238730, -105.2204629476320719 ) ) ;
#4696 = CARTESIAN_POINT ( 'NONE',  ( -20.99418893176411416, 178.7017074851977156, -124.8287954103437301 ) ) ;
#4697 = ORIENTED_EDGE ( 'NONE', *, *, #8310, .F. ) ;
#4698 = LINE ( 'NONE', #4438, #11123 ) ;
#4699 = CIRCLE ( 'NONE', #9621, 5.000000000000115463 ) ;
#4700 = ORIENTED_EDGE ( 'NONE', *, *, #2760, .F. ) ;
#4701 = CARTESIAN_POINT ( 'NONE',  ( -991.8293279264787543, 119.7328159579555091, -113.1262384684096673 ) ) ;
#4702 = ORIENTED_EDGE ( 'NONE', *, *, #8310, .T. ) ;
#4703 = AXIS2_PLACEMENT_3D ( 'NONE', #3661, #11331, #901 ) ;
#4704 = ORIENTED_EDGE ( 'NONE', *, *, #10020, .T. ) ;
#4705 = DIRECTION ( 'NONE',  ( -0.3117078928809153826, -1.979053562451413181E-14, -0.9501779778103363050 ) ) ;
#4706 = PLANE ( 'NONE',  #12225 ) ;
#4707 = CARTESIAN_POINT ( 'NONE',  ( -952.9945178120615310, 87.05516224832936700, -154.8742214401229660 ) ) ;
#4708 = ADVANCED_FACE ( 'NONE', ( #7088 ), #11732, .F. ) ;
#4709 = DIRECTION ( 'NONE',  ( 0.000000000000000000, 1.773410419504194611E-14, -1.000000000000000000 ) ) ;
#4710 = FACE_OUTER_BOUND ( 'NONE', #2773, .T. ) ;
#4711 = CARTESIAN_POINT ( 'NONE',  ( -1065.000000000007731, 93.55451860843886891, -152.5758913445290830 ) ) ;
#4712 = VERTEX_POINT ( 'NONE', #5921 ) ;
#4713 = CARTESIAN_POINT ( 'NONE',  ( -373.3728075979055347, 98.29427327314448348, -136.3749942106433366 ) ) ;
#4714 = VERTEX_POINT ( 'NONE', #6163 ) ;
#4715 = CARTESIAN_POINT ( 'NONE',  ( -1055.782959745576591, 85.17781532426890578, -154.2940595301287203 ) ) ;
#4716 = CARTESIAN_POINT ( 'NONE',  ( 19.85038338882363718, 181.0937693555581802, -127.1232350078937969 ) ) ;
#4717 = AXIS2_PLACEMENT_3D ( 'NONE', #3487, #8335, #11037 ) ;
#4718 = ADVANCED_BREP_SHAPE_REPRESENTATION ( '', ( #11906, #11957 ), #5648 ) ;
#4719 = VERTEX_POINT ( 'NONE', #10673 ) ;
#4720 = CIRCLE ( 'NONE', #6094, 7.500000000000007105 ) ;
#4721 = CARTESIAN_POINT ( 'NONE',  ( -828.1678681009909724, 81.16376924194530318, -144.6638077543062479 ) ) ;
#4722 = CARTESIAN_POINT ( 'NONE',  ( -19.95815963485732425, 182.4283802827153806, -125.9807797667228897 ) ) ;
#4723 = VERTEX_POINT ( 'NONE', #1460 ) ;
#4724 = CARTESIAN_POINT ( 'NONE',  ( -374.8265083808032045, 76.03942901340127491, -143.8108696807164790 ) ) ;
#4725 = LINE ( 'NONE', #5817, #5195 ) ;
#4726 = CARTESIAN_POINT ( 'NONE',  ( -384.2251555493538717, 74.58855242484294479, -106.1017844575084439 ) ) ;
#4727 = EDGE_CURVE ( 'NONE', #3651, #4474, #11287, .T. ) ;
#4728 = LINE ( 'NONE', #11220, #11006 ) ;
#4729 = AXIS2_PLACEMENT_3D ( 'NONE', #7716, #1180, #2964 ) ;
#4730 = ADVANCED_FACE ( 'NONE', ( #2274 ), #1230, .F. ) ;
#4731 = DIRECTION ( 'NONE',  ( 0.000000000000000000, 0.000000000000000000, -1.000000000000000000 ) ) ;
#4732 = DIRECTION ( 'NONE',  ( 0.000000000000000000, 0.000000000000000000, 1.000000000000000000 ) ) ;
#4733 = PRESENTATION_LAYER_ASSIGNMENT (  '', '', ( #7493 ) ) ;
#4734 = CARTESIAN_POINT ( 'NONE',  ( -996.5513353153756952, 56.29506814688433280, -99.57582448894517313 ) ) ;
#4735 = CARTESIAN_POINT ( 'NONE',  ( -795.0000000000043201, 82.00000000000039790, -124.6807709998041105 ) ) ;
#4736 = DIRECTION ( 'NONE',  ( 0.000000000000000000, 1.000000000000000000, 0.000000000000000000 ) ) ;
#4737 = CARTESIAN_POINT ( 'NONE',  ( -1032.644706488202019, 45.21923725197559207, -130.5712005305405228 ) ) ;
#4738 = CARTESIAN_POINT ( 'NONE',  ( -822.2160636604419324, 83.41847921025930646, -144.6308011508170352 ) ) ;
#4739 = ORIENTED_EDGE ( 'NONE', *, *, #4401, .F. ) ;
#4740 = CARTESIAN_POINT ( 'NONE',  ( -827.8097080315036465, 81.71711720835109816, -144.6806456489624395 ) ) ;
#4741 = CARTESIAN_POINT ( 'NONE',  ( -374.0007123233734774, 93.82451216013637918, -97.86852803052812533 ) ) ;
#4742 = ORIENTED_EDGE ( 'NONE', *, *, #8278, .T. ) ;
#4743 = CYLINDRICAL_SURFACE ( 'NONE', #8243, 7.500000000000007105 ) ;
#4744 = CARTESIAN_POINT ( 'NONE',  ( -1032.260242496269029, 61.00429285198274698, -99.57582448894517313 ) ) ;
#4745 = EDGE_CURVE ( 'NONE', #3812, #4910, #11617, .T. ) ;
#4746 = FACE_OUTER_BOUND ( 'NONE', #9447, .T. ) ;
#4747 = CIRCLE ( 'NONE', #1569, 57.99999999999999289 ) ;
#4748 = EDGE_CURVE ( 'NONE', #3744, #5923, #3249, .T. ) ;
#4749 = EDGE_LOOP ( 'NONE', ( #1424, #1005, #10893, #5530 ) ) ;
#4750 = CARTESIAN_POINT ( 'NONE',  ( -374.0392471180470011, 93.65555499067784240, -97.72940670563750132 ) ) ;
#4751 = VERTEX_POINT ( 'NONE', #6966 ) ;
#4752 = EDGE_CURVE ( 'NONE', #3398, #12119, #6042, .T. ) ;
#4753 = CARTESIAN_POINT ( 'NONE',  ( 0.01899995639453613133, -8.236198097127180873, -3.734486434573621061 ) ) ;
#4754 = FACE_OUTER_BOUND ( 'NONE', #8581, .T. ) ;
#4755 = CARTESIAN_POINT ( 'NONE',  ( -19.98141544511310386, 181.2666267236099884, -123.6015590193429858 ) ) ;
#4756 = ORIENTED_EDGE ( 'NONE', *, *, #4258, .F. ) ;
#4757 = CARTESIAN_POINT ( 'NONE',  ( -120.8820948793972434, 0.000000000000000000, -186.6989091883324363 ) ) ;
#4758 = DIRECTION ( 'NONE',  ( 0.000000000000000000, 0.000000000000000000, 1.000000000000000000 ) ) ;
#4759 = CARTESIAN_POINT ( 'NONE',  ( 0.000000000000000000, -6.000000000000000000, -126.4213562373094959 ) ) ;
#4760 = CARTESIAN_POINT ( 'NONE',  ( -926.8105964072267398, 116.1567348237267083, -146.0307792196442733 ) ) ;
#4761 = VECTOR ( 'NONE', #10726, 1000.000000000000000 ) ;
#4762 = CARTESIAN_POINT ( 'NONE',  ( 56.53599999999998715, 0.000000000000000000, 0.000000000000000000 ) ) ;
#4763 = DIRECTION ( 'NONE',  ( 0.000000000000000000, -1.156482317317870246E-16, 1.000000000000000000 ) ) ;
#4764 = ORIENTED_EDGE ( 'NONE', *, *, #5752, .T. ) ;
#4765 = DIRECTION ( 'NONE',  ( 0.000000000000000000, 0.000000000000000000, -1.000000000000000000 ) ) ;
#4766 = CARTESIAN_POINT ( 'NONE',  ( -371.5064087246056488, 103.8442247300971530, -141.3454260814483519 ) ) ;
#4767 = PRODUCT ( 'Bending Angle Gauge Plate', 'Bending Angle Gauge Plate', '', ( #6890 ) ) ;
#4768 = ORIENTED_EDGE ( 'NONE', *, *, #1014, .F. ) ;
#4769 = CARTESIAN_POINT ( 'NONE',  ( -1017.840614713428863, 119.3387310954208118, -130.5712005305402954 ) ) ;
#4770 = DIRECTION ( 'NONE',  ( 0.000000000000000000, 0.000000000000000000, 1.000000000000000000 ) ) ;
#4771 = ORIENTED_EDGE ( 'NONE', *, *, #2605, .F. ) ;
#4772 = VECTOR ( 'NONE', #10044, 1000.000000000000000 ) ;
#4773 = FACE_OUTER_BOUND ( 'NONE', #7615, .T. ) ;
#4774 = ORIENTED_EDGE ( 'NONE', *, *, #9688, .T. ) ;
#4775 = CARTESIAN_POINT ( 'NONE',  ( 20.82193910853440855, 179.1472446959528213, -123.7577175453547085 ) ) ;
#4776 = DIRECTION ( 'NONE',  ( 0.000000000000000000, 0.000000000000000000, 1.000000000000000000 ) ) ;
#4777 = DIRECTION ( 'NONE',  ( 0.000000000000000000, 0.000000000000000000, 1.000000000000000000 ) ) ;
#4778 = CARTESIAN_POINT ( 'NONE',  ( -1024.641217300042399, 73.20632742167555307, -152.5758913445296230 ) ) ;
#4779 = VECTOR ( 'NONE', #7101, 1000.000000000000000 ) ;
#4780 = CARTESIAN_POINT ( 'NONE',  ( -374.6843874209988599, 75.16053358314040622, -153.7112566340306046 ) ) ;
#4781 = DIRECTION ( 'NONE',  ( 0.000000000000000000, -1.669238443041288415E-16, 1.000000000000000000 ) ) ;
#4782 = CARTESIAN_POINT ( 'NONE',  ( -384.7852612105363619, 78.04101542915444156, -105.0654598586175581 ) ) ;
#4783 = DIRECTION ( 'NONE',  ( 1.000000000000000000, 0.000000000000000000, 0.000000000000000000 ) ) ;
#4784 = ORIENTED_EDGE ( 'NONE', *, *, #1792, .F. ) ;
#4785 = CIRCLE ( 'NONE', #3376, 7.500000000000012434 ) ;
#4786 = EDGE_CURVE ( 'NONE', #1233, #7767, #5567, .T. ) ;
#4787 = CYLINDRICAL_SURFACE ( 'NONE', #1909, 7.500000000000007994 ) ;
#4788 = DIRECTION ( 'NONE',  ( 2.040851148208007875E-17, -1.000000000000000000, -0.000000000000000000 ) ) ;
#4789 = ADVANCED_FACE ( 'NONE', ( #10981 ), #3425, .F. ) ;
#4790 = CARTESIAN_POINT ( 'NONE',  ( -1032.113539130918525, 67.34854938887495734, -96.78565065507952170 ) ) ;
#4791 = CARTESIAN_POINT ( 'NONE',  ( -828.8285638327243987, 78.67432280806561096, -104.9592124606052863 ) ) ;
#4792 = VERTEX_POINT ( 'NONE', #4370 ) ;
#4793 = CARTESIAN_POINT ( 'NONE',  ( -381.3501251071949696, 66.06991304680765609, -112.5745157944540864 ) ) ;
#4794 = ORIENTED_EDGE ( 'NONE', *, *, #2374, .T. ) ;
#4795 = EDGE_CURVE ( 'NONE', #10372, #1988, #1816, .T. ) ;
#4796 = APPLICATION_PROTOCOL_DEFINITION ( 'draft international standard', 'automotive_design', 1998, #11592 ) ;
#4797 = CARTESIAN_POINT ( 'NONE',  ( -372.8708942284384307, 99.15106812072066589, -101.9386899173519936 ) ) ;
#4798 = ORIENTED_EDGE ( 'NONE', *, *, #7505, .F. ) ;
#4799 = CARTESIAN_POINT ( 'NONE',  ( -1062.923339974269538, 49.86928741160662071, -113.1262384684094968 ) ) ;
#4800 = CARTESIAN_POINT ( 'NONE',  ( -87.04832655144203102, 0.000000000000000000, -210.4289243767376831 ) ) ;
#4801 = LINE ( 'NONE', #1100, #3629 ) ;
#4802 = CARTESIAN_POINT ( 'NONE',  ( 154.5043356068769071, 0.000000000000000000, -102.0666613060171386 ) ) ;
#4803 = FACE_BOUND ( 'NONE', #11708, .T. ) ;
#4804 = ADVANCED_FACE ( 'NONE', ( #1646 ), #3365, .T. ) ;
#4805 = ORIENTED_EDGE ( 'NONE', *, *, #1246, .T. ) ;
#4806 = FACE_OUTER_BOUND ( 'NONE', #7673, .T. ) ;
#4807 = CARTESIAN_POINT ( 'NONE',  ( -371.7612374550235472, 103.0478591256022014, -106.7472349355403480 ) ) ;
#4808 = CIRCLE ( 'NONE', #3214, 7.500000000000007105 ) ;
#4809 = ORIENTED_EDGE ( 'NONE', *, *, #2065, .T. ) ;
#4810 = PLANE ( 'NONE',  #5253 ) ;
#4811 = CARTESIAN_POINT ( 'NONE',  ( -1024.722591077094876, 118.3980260646368379, -130.5712005305404944 ) ) ;
#4812 = CYLINDRICAL_SURFACE ( 'NONE', #3117, 7.500000000000007105 ) ;
#4813 = CIRCLE ( 'NONE', #11135, 7.500000000000007105 ) ;
#4814 = CARTESIAN_POINT ( 'NONE',  ( -1065.000000000003411, 111.6133447792289104, -118.7903414690678972 ) ) ;
#4815 = ORIENTED_EDGE ( 'NONE', *, *, #8680, .F. ) ;
#4816 = EDGE_CURVE ( 'NONE', #5163, #7478, #5475, .T. ) ;
#4817 = DIRECTION ( 'NONE',  ( -1.000000000000000000, 0.000000000000000000, 0.000000000000000000 ) ) ;
#4818 = DIRECTION ( 'NONE',  ( 0.9501779778103254248, 0.000000000000000000, 0.3117078928809486338 ) ) ;
#4819 = DIRECTION ( 'NONE',  ( -1.000000000000000000, 0.000000000000000000, 0.000000000000000000 ) ) ;
#4820 = CYLINDRICAL_SURFACE ( 'NONE', #1660, 7.500000000000007994 ) ;
#4821 = ORIENTED_EDGE ( 'NONE', *, *, #6369, .F. ) ;
#4822 = AXIS2_PLACEMENT_3D ( 'NONE', #979, #11355, #4858 ) ;
#4823 = AXIS2_PLACEMENT_3D ( 'NONE', #9717, #5069, #5011 ) ;
#4824 = CARTESIAN_POINT ( 'NONE',  ( -1025.296800000958683, 108.9225844456048691, -146.0307792196446144 ) ) ;
#4825 = FACE_BOUND ( 'NONE', #1576, .T. ) ;
#4826 = EDGE_LOOP ( 'NONE', ( #849, #11112, #3459, #7940 ) ) ;
#4827 = ORIENTED_EDGE ( 'NONE', *, *, #9479, .T. ) ;
#4828 = CIRCLE ( 'NONE', #6407, 7.500000000000007105 ) ;
#4829 = CARTESIAN_POINT ( 'NONE',  ( -21.03937020940231051, 181.6480601768998895, -125.3115690614735911 ) ) ;
#4830 = VECTOR ( 'NONE', #10348, 1000.000000000000000 ) ;
#4831 = CARTESIAN_POINT ( 'NONE',  ( -11.89695805161369080, 180.2041921146325478, -183.6976696918626999 ) ) ;
#4832 = CARTESIAN_POINT ( 'NONE',  ( -795.0000000000002274, 56.89504896194490868, -141.4553492942756350 ) ) ;
#4833 = EDGE_LOOP ( 'NONE', ( #2154, #2687, #1871, #8872 ) ) ;
#4834 = CARTESIAN_POINT ( 'NONE',  ( -374.9996141881664471, 82.89264451733117767, -154.6796575120754653 ) ) ;
#4835 = LINE ( 'NONE', #131, #9554 ) ;
#4836 = CARTESIAN_POINT ( 'NONE',  ( -382.4095633919862962, 68.53572743257521438, -109.8882287899762389 ) ) ;
#4837 = DIRECTION ( 'NONE',  ( -1.000000000000000000, -0.000000000000000000, 0.000000000000000000 ) ) ;
#4838 = ORIENTED_EDGE ( 'NONE', *, *, #9507, .T. ) ;
#4839 = AXIS2_PLACEMENT_3D ( 'NONE', #6353, #10422, #1732 ) ;
#4840 = ORIENTED_EDGE ( 'NONE', *, *, #7473, .F. ) ;
#4841 = CARTESIAN_POINT ( 'NONE',  ( 19.97899957837033824, 177.8194711809319415, -125.6095969703938096 ) ) ;
#4842 = CARTESIAN_POINT ( 'NONE',  ( -853.8938961404153360, 37.86297855175766358, -103.3307627799636776 ) ) ;
#4843 = CARTESIAN_POINT ( 'NONE',  ( 7.653191805780027529E-16, 138.9999999999999716, -126.4213562373094959 ) ) ;
#4844 = B_SPLINE_CURVE_WITH_KNOTS ( 'NONE', 3,
 ( #9654, #4886, #2178, #181, #3904, #3963, #7732, #2115, #11572, #4094, #1195, #11385, #3035, #243, #4028, #3100, #9712, #5005, #7864, #11638, #5186, #7234, #4331, #10069, #6059, #8893, #8045, #10870, #9826, #4151, #4207, #1366, #7107, #11811, #9892, #2357, #7924, #7982, #3327, #6984, #2406, #10757, #7044, #1427, #5131, #3208, #6245, #11693, #9139, #10999 ),
 .UNSPECIFIED., .F., .F.,
 ( 4, 2, 2, 2, 2, 2, 2, 2, 2, 2, 2, 2, 2, 2, 2, 2, 2, 2, 2, 2, 2, 2, 2, 2, 4 ),
 ( 0.006558949033259317725, 0.01013307393990397348, 0.01192013639322624802, 0.01370719884654851908, 0.01728132375319304040, 0.01906838620651532534, 0.02085544865983761376, 0.02442957356648214895, 0.02621663601980439226, 0.02800369847312663557, 0.03157782337977111525, 0.03336488583309336203, 0.03515194828641559494, 0.03872607319306003298, 0.04051313564638227283, 0.04230019809970450573, 0.04587432300634893684, 0.04766138545967119056, 0.04944844791299343734, 0.05302257281963791702, 0.05480963527296017768, 0.05659669772628243140, 0.05838376017960469205, 0.06017082263292695271, 0.06374494753957145321 ),
 .UNSPECIFIED. ) ;
#4845 = ORIENTED_EDGE ( 'NONE', *, *, #3334, .T. ) ;
#4846 = CARTESIAN_POINT ( 'NONE',  ( -384.6667163751908447, 76.99832943347863079, -105.2798939677049503 ) ) ;
#4847 = DIRECTION ( 'NONE',  ( 0.000000000000000000, 0.000000000000000000, 1.000000000000000000 ) ) ;
#4848 = EDGE_LOOP ( 'NONE', ( #7835, #10364, #3038, #5376 ) ) ;
#4849 = EDGE_CURVE ( 'NONE', #3585, #3288, #223, .T. ) ;
#4850 = ORIENTED_EDGE ( 'NONE', *, *, #5479, .F. ) ;
#4851 = CARTESIAN_POINT ( 'NONE',  ( -1017.027421246622112, 56.01181809833683900, -113.1262384684095537 ) ) ;
#4852 = CYLINDRICAL_SURFACE ( 'NONE', #11488, 7.500000000000013323 ) ;
#4853 = DIRECTION ( 'NONE',  ( 0.000000000000000000, 0.000000000000000000, 1.000000000000000000 ) ) ;
#4854 = PLANE ( 'NONE',  #6567 ) ;
#4855 = AXIS2_PLACEMENT_3D ( 'NONE', #12023, #8331, #5596 ) ;
#4856 = CARTESIAN_POINT ( 'NONE',  ( -1060.958858734054957, 107.4804882715807963, -107.9061927053325007 ) ) ;
#4857 = CARTESIAN_POINT ( 'NONE',  ( -59.99999999999998579, 12.00000000000001421, -126.4213562373090696 ) ) ;
#4858 = DIRECTION ( 'NONE',  ( -1.000000000000000000, 0.000000000000000000, 0.000000000000000000 ) ) ;
#4859 = VERTEX_POINT ( 'NONE', #12033 ) ;
#4860 = ORIENTED_EDGE ( 'NONE', *, *, #1726, .T. ) ;
#4862 = EDGE_CURVE ( 'NONE', #7231, #4601, #3545, .T. ) ;
#4861 = CARTESIAN_POINT ( 'NONE',  ( -951.7027691703317487, 118.7449601027236241, -107.9061927053324581 ) ) ;
#4863 = AXIS2_PLACEMENT_3D ( 'NONE', #11397, #9481, #2068 ) ;
#4864 = CARTESIAN_POINT ( 'NONE',  ( 144.0488662551573782, 12.00000000000000000, -139.4077238332702109 ) ) ;
#4865 = DIRECTION ( 'NONE',  ( 0.000000000000000000, 0.000000000000000000, 1.000000000000000000 ) ) ;
#4866 = ADVANCED_FACE ( 'NONE', ( #12170 ), #11241, .F. ) ;
#4867 = CARTESIAN_POINT ( 'NONE',  ( -926.5138833012647410, 125.7648744980332225, -124.6807709998040394 ) ) ;
#4868 = VERTEX_POINT ( 'NONE', #8406 ) ;
#4869 = AXIS2_PLACEMENT_3D ( 'NONE', #12031, #11103, #1778 ) ;
#4870 = DIRECTION ( 'NONE',  ( 0.000000000000000000, 1.000000000000000000, 0.000000000000000000 ) ) ;
#4871 = FACE_BOUND ( 'NONE', #730, .T. ) ;
#4872 = SHAPE_REPRESENTATION ( 'pin to fix handle', ( #11957 ), #10774 ) ;
#4873 = DIRECTION ( 'NONE',  ( 0.000000000000000000, 1.000000000000000000, 0.000000000000000000 ) ) ;
#4874 = DIRECTION ( 'NONE',  ( 0.000000000000000000, 0.000000000000000000, 1.000000000000000000 ) ) ;
#4875 = ORIENTED_EDGE ( 'NONE', *, *, #9843, .T. ) ;
#4876 = CARTESIAN_POINT ( 'NONE',  ( -1037.337636019037518, 116.9882293220590270, -126.6442663926289640 ) ) ;
#4877 = DIRECTION ( 'NONE',  ( 3.061276722312011504E-17, -1.000000000000000000, -0.000000000000000000 ) ) ;
#4878 = CIRCLE ( 'NONE', #3699, 7.500000000000007994 ) ;
#4879 = ADVANCED_FACE ( 'NONE', ( #2768 ), #10300, .T. ) ;
#4880 = AXIS2_PLACEMENT_3D ( 'NONE', #5955, #1260, #1380 ) ;
#4881 = ADVANCED_FACE ( 'NONE', ( #9315 ), #10632, .F. ) ;
#4882 = FACE_BOUND ( 'NONE', #11100, .T. ) ;
#4883 = ORIENTED_EDGE ( 'NONE', *, *, #11843, .F. ) ;
#4884 = ORIENTED_EDGE ( 'NONE', *, *, #1686, .T. ) ;
#4885 = EDGE_CURVE ( 'NONE', #3207, #10076, #1609, .T. ) ;
#4886 = CARTESIAN_POINT ( 'NONE',  ( -380.0073966942719039, 100.5504690541876442, -132.2504864982372226 ) ) ;
#4887 = CARTESIAN_POINT ( 'NONE',  ( -1057.036663358150690, 58.23757105449725913, -149.7857175106634884 ) ) ;
#4888 = ORIENTED_EDGE ( 'NONE', *, *, #1114, .T. ) ;
#4889 = MECHANICAL_DESIGN_GEOMETRIC_PRESENTATION_REPRESENTATION (  '', ( #1159 ), #1349 ) ;
#4890 = CARTESIAN_POINT ( 'NONE',  ( -384.9269939781261201, 79.69860309749668659, -144.5506590107445390 ) ) ;
#4891 = CARTESIAN_POINT ( 'NONE',  ( 1.387778780781445676E-14, 11.99999999999999645, 133.9213562373095101 ) ) ;
#4892 = DIRECTION ( 'NONE',  ( -2.081668171172161734E-17, -4.930380657631307143E-31, 1.000000000000000000 ) ) ;
#4893 = CARTESIAN_POINT ( 'NONE',  ( -1014.004070199769671, 54.58258344709567922, -136.2353035311988947 ) ) ;
#4894 = EDGE_CURVE ( 'NONE', #3503, #8380, #2401, .T. ) ;
#4895 = VECTOR ( 'NONE', #5220, 1000.000000000000000 ) ;
#4896 = CARTESIAN_POINT ( 'NONE',  ( 4.216865464401061553E-15, 168.0000000000000000, -124.6807709998038405 ) ) ;
#4897 = STYLED_ITEM ( 'NONE', ( #6252 ), #8194 ) ;
#4898 = ORIENTED_EDGE ( 'NONE', *, *, #8278, .F. ) ;
#4899 = DIRECTION ( 'NONE',  ( -0.000000000000000000, 1.000000000000000000, 7.930164461608263644E-17 ) ) ;
#4900 = CARTESIAN_POINT ( 'NONE',  ( -1032.503061859599256, 50.81309391744463255, -107.9061927053326428 ) ) ;
#4901 = CARTESIAN_POINT ( 'NONE',  ( 3.133148353965215262E-13, 152.0000000000000000, -103.9213562373094817 ) ) ;
#4902 = CARTESIAN_POINT ( 'NONE',  ( -379.7887390581964837, 100.9343252097582564, -131.1221473163307678 ) ) ;
#4903 = ORIENTED_EDGE ( 'NONE', *, *, #199, .T. ) ;
#4904 = CIRCLE ( 'NONE', #3935, 1.500000000000000666 ) ;
#4905 = ORIENTED_EDGE ( 'NONE', *, *, #3593, .T. ) ;
#4906 = DIRECTION ( 'NONE',  ( 0.7071067811865479058, -0.000000000000000000, 0.7071067811865472397 ) ) ;
#4907 = VERTEX_POINT ( 'NONE', #4999 ) ;
#4908 = VECTOR ( 'NONE', #11616, 1000.000000000000000 ) ;
#4909 = PRODUCT_CONTEXT ( 'NONE', #9295, 'mechanical' ) ;
#4910 = VERTEX_POINT ( 'NONE', #5934 ) ;
#4911 = CARTESIAN_POINT ( 'NONE',  ( -957.0819499390169085, 50.45265437475560333, -113.1262384684095537 ) ) ;
#4912 = CYLINDRICAL_SURFACE ( 'NONE', #9238, 7.500000000000007105 ) ;
#4913 = CARTESIAN_POINT ( 'NONE',  ( -28.53314250459843038, 180.2041921146317236, -137.7978499286131751 ) ) ;
#4914 = FACE_OUTER_BOUND ( 'NONE', #1133, .T. ) ;
#4915 = AXIS2_PLACEMENT_3D ( 'NONE', #2656, #7485, #2786 ) ;
#4916 = UNCERTAINTY_MEASURE_WITH_UNIT (LENGTH_MEASURE( 1.000000000000000082E-05 ), #3090, 'distance_accuracy_value', 'NONE');
#4917 = CARTESIAN_POINT ( 'NONE',  ( 9.371890508914830252E-13, -6.000000000000005329, -36.42135623730949590 ) ) ;
#4918 = CARTESIAN_POINT ( 'NONE',  ( -21.04069087917613956, 178.7655007512674104, -125.3296589603482261 ) ) ;
#4919 = CARTESIAN_POINT ( 'NONE',  ( 120.8820948793965186, 0.000000000000000000, -186.6989091883332890 ) ) ;
#4920 = EDGE_LOOP ( 'NONE', ( #9673, #5871 ) ) ;
#4921 = CARTESIAN_POINT ( 'NONE',  ( -375.0000000000000568, 81.99999999999994316, -154.6807709998039115 ) ) ;
#4922 = AXIS2_PLACEMENT_3D ( 'NONE', #9968, #7060, #10831 ) ;
#4923 = VECTOR ( 'NONE', #5845, 1000.000000000000000 ) ;
#4924 = VERTEX_POINT ( 'NONE', #11567 ) ;
#4925 = CARTESIAN_POINT ( 'NONE',  ( -955.0423082396529253, 101.0797422464698059, -96.78565065507901011 ) ) ;
#4926 = CARTESIAN_POINT ( 'NONE',  ( -954.1708249681001917, 122.1961423320944249, -136.2353035311976157 ) ) ;
#4927 = DIRECTION ( 'NONE',  ( -0.000000000000000000, -1.000000000000000000, -0.000000000000000000 ) ) ;
#4928 = ADVANCED_FACE ( 'NONE', ( #9704 ), #1824, .T. ) ;
#4929 = CARTESIAN_POINT ( 'NONE',  ( -1021.743962174751232, 119.2557508373789403, -124.6807709998040110 ) ) ;
#4930 = ORIENTED_EDGE ( 'NONE', *, *, #5776, .T. ) ;
#4931 = FACE_OUTER_BOUND ( 'NONE', #6476, .T. ) ;
#4932 = EDGE_CURVE ( 'NONE', #11612, #5315, #4021, .T. ) ;
#4933 = DIRECTION ( 'NONE',  ( 0.000000000000000000, -1.000000000000000000, -7.930164461608263644E-17 ) ) ;
#4934 = FACE_BOUND ( 'NONE', #8354, .T. ) ;
#4935 = CARTESIAN_POINT ( 'NONE',  ( -1031.086615573508880, 111.8776252365151009, -141.4553492942759760 ) ) ;
#4936 = CARTESIAN_POINT ( 'NONE',  ( -818.8285638327243987, 78.67432280806558254, -94.73795703228648790 ) ) ;
#4937 = CARTESIAN_POINT ( 'NONE',  ( 0.8038475772931109598, -5.196152422707023710, -9.000000000000001776 ) ) ;
#4938 =( NAMED_UNIT ( * ) PLANE_ANGLE_UNIT ( ) SI_UNIT ( $, .RADIAN. ) );
#4939 = EDGE_LOOP ( 'NONE', ( #12216, #9649 ) ) ;
#4940 = DIRECTION ( 'NONE',  ( 0.000000000000000000, -1.156482317317870246E-16, 1.000000000000000000 ) ) ;
#4941 = CARTESIAN_POINT ( 'NONE',  ( -904.2101318205999405, 125.2895275102983419, -124.6807709998041531 ) ) ;
#4942 = EDGE_CURVE ( 'NONE', #6687, #3591, #10498, .T. ) ;
#4943 = CARTESIAN_POINT ( 'NONE',  ( -1037.461794897090840, 110.6138330393710731, -141.4553492942763171 ) ) ;
#4944 = FACE_BOUND ( 'NONE', #1687, .T. ) ;
#4945 = ORIENTED_EDGE ( 'NONE', *, *, #10768, .F. ) ;
#4946 = ORIENTED_EDGE ( 'NONE', *, *, #654, .T. ) ;
#4947 =( BOUNDED_SURFACE ( )  B_SPLINE_SURFACE ( 3, 2, ( 
 ( #4455, #11993, #9015 ),
 ( #12055, #7300, #3567 ),
 ( #551, #11866, #3382 ),
 ( #11064, #4522, #2589 ),
 ( #7358, #6361, #10133 ),
 ( #11128, #10940, #5502 ),
 ( #9275, #8360, #51 ),
 ( #878, #3706, #1061 ),
 ( #9580, #6551, #1120 ),
 ( #11200, #7603, #10318 ),
 ( #10267, #1798, #7483 ),
 ( #5622, #294, #10622 ),
 ( #4193, #4140, #9880 ),
 ( #2342, #5860, #7912 ),
 ( #6973, #10742, #9635 ),
 ( #7718, #6048, #3952 ),
 ( #170, #1354, #7784 ),
 ( #11183, #8473, #7529 ),
 ( #3693, #6660, #8346 ),
 ( #10253, #9257, #12234 ),
 ( #4807, #12177, #6718 ),
 ( #36, #5610, #10430 ),
 ( #2832, #1723, #4569 ),
 ( #2896, #1971, #11419 ),
 ( #5483, #5729, #10307 ),
 ( #1047, #7470, #8415 ),
 ( #11296, #801, #102 ),
 ( #2707, #5670, #2775 ),
 ( #9446, #9504, #5550 ),
 ( #4750, #1906, #9324 ),
 ( #8522, #9387, #866 ),
 ( #7648, #3813, #7588 ),
 ( #11358, #4636, #6776 ),
 ( #9802, #5103, #6842 ),
 ( #8643, #11483, #3016 ),
 ( #5273, #4243, #6097 ),
 ( #10845, #3355, #5213 ),
 ( #517, #3411, #1635 ),
 ( #8262, #2497, #1575 ),
 ( #8613, #2872, #8553 ),
 ( #3969, #2121, #7623 ),
 ( #8732, #10583, #132 ),
 ( #8502, #5880, #6632 ),
 ( #72, #2984, #4782 ),
 ( #11391, #8, #1882 ),
 ( #3536, #3784, #2803 ),
 ( #3850, #3041, #9659 ),
 ( #10397, #2930, #4726 ),
 ( #4955, #6746, #6690 ),
 ( #10466, #7559, #5646 ),
 ( #7329, #1940, #6575 ),
 ( #3910, #1200, #7739 ),
 ( #5702, #7684, #2059 ),
 ( #11274, #9476, #2001 ),
 ( #8679, #10340, #5818 ),
 ( #9419, #5758, #9534 ),
 ( #1079, #6812, #4836 ),
 ( #11453, #9596, #187 ),
 ( #11513, #4211, #6876 ),
 ( #9958, #11817, #5246 ),
 ( #7988, #5945, #8791 ),
 ( #11761, #11699, #4098 ),
 ( #3161, #10761, #2295 ),
 ( #6065, #9832, #6151 ),
 ( #7019, #9919, #7139 ),
 ( #1395, #1449, #4242 ) ),
 .UNSPECIFIED., .F., .F., .F. ) 
 B_SPLINE_SURFACE_WITH_KNOTS ( ( 4, 2, 2, 2, 2, 2, 2, 2, 2, 2, 2, 2, 2, 2, 2, 2, 2, 2, 2, 2, 2, 2, 2, 2, 2, 2, 2, 2, 2, 2, 2, 2, 4 ),
 ( 3, 3 ),
 ( 0.000000000000000000, 0.005905868208427481753, 0.008858802312641222629, 0.01181173641685496351, 0.01771760462528244526, 0.01919407167738931830, 0.02067053872949618787, 0.02362347283370992701, 0.02657640693792366615, 0.02805287399003053572, 0.02952934104213740876, 0.03543520925056489052, 0.03838814335477863660, 0.03986461040688550617, 0.04134107745899237574, 0.04724694566741985402, 0.04872341271952672359, 0.05019987977163359316, 0.05315281387584733230, 0.05905868208427481753, 0.06053514913638169403, 0.06201161618848856361, 0.06496455029270230275, 0.06791748439691604189, 0.06939395144902291146, 0.07087041850112978103, 0.07677628670955727319, 0.07825275376166414276, 0.07972922081377101233, 0.08268215491798475147, 0.08858802312641222976, 0.09154095723062596890, 0.09449389133483970804 ),
 ( 0.000000000000000000, 1.000000000000000000 ),
 .UNSPECIFIED. ) 
 GEOMETRIC_REPRESENTATION_ITEM ( )  RATIONAL_B_SPLINE_SURFACE ( (
 ( 1.000000000000000000, 0.8173438319342977154, 1.000000000000000000),
 ( 1.000000000000000000, 0.8219731356928380306, 1.000000000000000000),
 ( 1.000000000000000000, 0.8253030949534714278, 1.000000000000000000),
 ( 1.000000000000000000, 0.8281883099846812923, 1.000000000000000000),
 ( 1.000000000000000000, 0.8287982319878953730, 1.000000000000000000),
 ( 1.000000000000000000, 0.8292799412275436710, 1.000000000000000000),
 ( 1.000000000000000000, 0.8291455057931963468, 1.000000000000000000),
 ( 1.000000000000000000, 0.8276356789430494576, 1.000000000000000000),
 ( 1.000000000000000000, 0.8251732266201541321, 1.000000000000000000),
 ( 1.000000000000000000, 0.8204358190366770609, 1.000000000000000000),
 ( 1.000000000000000000, 0.8194051565372284518, 1.000000000000000000),
 ( 1.000000000000000000, 0.8171807861351056967, 1.000000000000000000),
 ( 1.000000000000000000, 0.8159873918869244847, 1.000000000000000000),
 ( 1.000000000000000000, 0.8122138746351555971, 1.000000000000000000),
 ( 1.000000000000000000, 0.8094285655643660427, 1.000000000000000000),
 ( 1.000000000000000000, 0.8033969199180073240, 1.000000000000000000),
 ( 1.000000000000000000, 0.8001503750370143608, 1.000000000000000000),
 ( 1.000000000000000000, 0.7949907125291132415, 1.000000000000000000),
 ( 1.000000000000000000, 0.7932225112627224739, 1.000000000000000000),
 ( 1.000000000000000000, 0.7895990428243180315, 1.000000000000000000),
 ( 1.000000000000000000, 0.7877388389179781347, 1.000000000000000000),
 ( 1.000000000000000000, 0.7783154489584510616, 1.000000000000000000),
 ( 1.000000000000000000, 0.7703989790022252038, 1.000000000000000000),
 ( 1.000000000000000000, 0.7585783171957931614, 1.000000000000000000),
 ( 1.000000000000000000, 0.7546473462006216826, 1.000000000000000000),
 ( 1.000000000000000000, 0.7488515224148959426, 1.000000000000000000),
 ( 1.000000000000000000, 0.7469324236575801690, 1.000000000000000000),
 ( 1.000000000000000000, 0.7431824754817925038, 1.000000000000000000),
 ( 1.000000000000000000, 0.7413476955835877069, 1.000000000000000000),
 ( 1.000000000000000000, 0.7324082410571595148, 1.000000000000000000),
 ( 1.000000000000000000, 0.7260035404487192867, 1.000000000000000000),
 ( 1.000000000000000000, 0.7194925012805183373, 1.000000000000000000),
 ( 1.000000000000000000, 0.7182652744297027825, 1.000000000000000000),
 ( 1.000000000000000000, 0.7159759613185773253, 1.000000000000000000),
 ( 1.000000000000000000, 0.7149113897941246076, 1.000000000000000000),
 ( 1.000000000000000000, 0.7120188864153280672, 1.000000000000000000),
 ( 1.000000000000000000, 0.7104833412027944384, 1.000000000000000000),
 ( 1.000000000000000000, 0.7071146405918344868, 1.000000000000000000),
 ( 1.000000000000000000, 0.7065236520918728447, 1.000000000000000000),
 ( 1.000000000000000000, 0.7079900934967895409, 1.000000000000000000),
 ( 1.000000000000000000, 0.7083941403342759457, 1.000000000000000000),
 ( 1.000000000000000000, 0.7094079449006509552, 1.000000000000000000),
 ( 1.000000000000000000, 0.7100184007272103415, 1.000000000000000000),
 ( 1.000000000000000000, 0.7121454404538102301, 1.000000000000000000),
 ( 1.000000000000000000, 0.7139577670361945128, 1.000000000000000000),
 ( 1.000000000000000000, 0.7182895641410933507, 1.000000000000000000),
 ( 1.000000000000000000, 0.7208090478352079389, 1.000000000000000000),
 ( 1.000000000000000000, 0.7250557726365194355, 1.000000000000000000),
 ( 1.000000000000000000, 0.7265534932289373637, 1.000000000000000000),
 ( 1.000000000000000000, 0.7296713736093599634, 1.000000000000000000),
 ( 1.000000000000000000, 0.7312892119586734685, 1.000000000000000000),
 ( 1.000000000000000000, 0.7396315842215842595, 1.000000000000000000),
 ( 1.000000000000000000, 0.7471097587475988844, 1.000000000000000000),
 ( 1.000000000000000000, 0.7568743091753726837, 1.000000000000000000),
 ( 1.000000000000000000, 0.7588483787671314040, 1.000000000000000000),
 ( 1.000000000000000000, 0.7628250640091223111, 1.000000000000000000),
 ( 1.000000000000000000, 0.7648239673428672836, 1.000000000000000000),
 ( 1.000000000000000000, 0.7707817864204414837, 1.000000000000000000),
 ( 1.000000000000000000, 0.7747203848179342600, 1.000000000000000000),
 ( 1.000000000000000000, 0.7862853007360839364, 1.000000000000000000),
 ( 1.000000000000000000, 0.7936618350787719711, 1.000000000000000000),
 ( 1.000000000000000000, 0.8036599604343283021, 1.000000000000000000),
 ( 1.000000000000000000, 0.8067667731041444634, 1.000000000000000000),
 ( 1.000000000000000000, 0.8124350975610165060, 1.000000000000000000),
 ( 1.000000000000000000, 0.8150032476531663406, 1.000000000000000000),
 ( 1.000000000000000000, 0.8172789612916436797, 1.000000000000000000) ) ) 
 REPRESENTATION_ITEM ( '' )  SURFACE ( )  );
#4948 = CARTESIAN_POINT ( 'NONE',  ( -820.7525053003688527, 74.71879621637260982, -106.0522004026988867 ) ) ;
#4949 = CARTESIAN_POINT ( 'NONE',  ( -902.0880155070129831, 62.23309906011792947, -141.4553492942754644 ) ) ;
#4950 = FACE_OUTER_BOUND ( 'NONE', #12207, .T. ) ;
#4951 = ORIENTED_EDGE ( 'NONE', *, *, #11986, .T. ) ;
#4952 = ADVANCED_FACE ( 'NONE', ( #5180 ), #7918, .F. ) ;
#4953 = CARTESIAN_POINT ( 'NONE',  ( -384.4245930906317881, 88.51370271557355807, -143.6368780726383250 ) ) ;
#4954 = DIRECTION ( 'NONE',  ( 1.000000000000000000, 0.000000000000000000, 0.000000000000000000 ) ) ;
#4955 = CARTESIAN_POINT ( 'NONE',  ( -374.2643749961815729, 71.87048632683526250, -96.99996408687380267 ) ) ;
#4956 = ORIENTED_EDGE ( 'NONE', *, *, #5915, .T. ) ;
#4957 = CARTESIAN_POINT ( 'NONE',  ( -1017.133222628203043, 54.07990892584120246, -130.5712005305404375 ) ) ;
#4958 = ORIENTED_EDGE ( 'NONE', *, *, #7435, .F. ) ;
#4959 = VERTEX_POINT ( 'NONE', #9761 ) ;
#4960 = CARTESIAN_POINT ( 'NONE',  ( -120.8820948793972434, 12.00000000000000000, -179.1989091883324363 ) ) ;
#4961 = VECTOR ( 'NONE', #9746, 1000.000000000000000 ) ;
#4962 = CARTESIAN_POINT ( 'NONE',  ( -1017.133222628208614, 54.07990892584129483, -118.7903414690683519 ) ) ;
#4963 = CARTESIAN_POINT ( 'NONE',  ( -19.87519864879851994, 178.8871479037923393, -126.9115732480538838 ) ) ;
#4964 = ORIENTED_EDGE ( 'NONE', *, *, #2893, .T. ) ;
#4965 = EDGE_CURVE ( 'NONE', #1219, #12001, #6919, .T. ) ;
#4966 = ORIENTED_EDGE ( 'NONE', *, *, #10682, .T. ) ;
#4967 = CARTESIAN_POINT ( 'NONE',  ( 0.000000000000000000, 0.000000000000000000, -264.6807709998040536 ) ) ;
#4968 = ORIENTED_EDGE ( 'NONE', *, *, #6853, .F. ) ;
#4969 = CARTESIAN_POINT ( 'NONE',  ( 0.000000000000000000, 0.000000000000000000, 0.000000000000000000 ) ) ;
#4970 = EDGE_LOOP ( 'NONE', ( #7452, #395, #1081, #10447 ) ) ;
#4971 = AXIS2_PLACEMENT_3D ( 'NONE', #1363, #8946, #3153 ) ;
#4972 = CARTESIAN_POINT ( 'NONE',  ( -854.0393178910176175, 26.93106345811105840, -113.1262384684097100 ) ) ;
#4973 = DIRECTION ( 'NONE',  ( -8.163404592832030268E-17, 1.000000000000000000, -0.000000000000000000 ) ) ;
#4974 = UNCERTAINTY_MEASURE_WITH_UNIT (LENGTH_MEASURE( 1.000000000000000082E-05 ), #8426, 'distance_accuracy_value', 'NONE');
#4975 = CARTESIAN_POINT ( 'NONE',  ( -1037.773541645229670, 93.34895244571353601, -96.78565065507908116 ) ) ;
#4976 = CIRCLE ( 'NONE', #5507, 45.00000000000001421 ) ;
#4977 = AXIS2_PLACEMENT_3D ( 'NONE', #11946, #7318, #1819 ) ;
#4978 = EDGE_LOOP ( 'NONE', ( #4995, #2678, #12060, #11832 ) ) ;
#4979 = CARTESIAN_POINT ( 'NONE',  ( -955.0000000000038654, 82.00000000000036948, -124.6807709998041673 ) ) ;
#4980 = VERTEX_POINT ( 'NONE', #9886 ) ;
#4981 = CARTESIAN_POINT ( 'NONE',  ( -955.3297122972882107, 93.84065249268854814, -95.06748246948001224 ) ) ;
#4982 = ORIENTED_EDGE ( 'NONE', *, *, #6350, .T. ) ;
#4983 = CARTESIAN_POINT ( 'NONE',  ( -852.9318753287220716, 113.3383058689776277, -141.4553492942764024 ) ) ;
#4984 = AXIS2_PLACEMENT_3D ( 'NONE', #633, #8001, #11712 ) ;
#4985 = DIRECTION ( 'NONE',  ( 0.000000000000000000, -1.156482317317870246E-16, 1.000000000000000000 ) ) ;
#4986 = CARTESIAN_POINT ( 'NONE',  ( -974.1288507787422759, 124.2142274477005657, -124.6807709998040110 ) ) ;
#4987 = ORIENTED_EDGE ( 'NONE', *, *, #7278, .F. ) ;
#4988 = CARTESIAN_POINT ( 'NONE',  ( 1.249585401188644101E-12, 164.0000000000000000, 1.078643762690527641 ) ) ;
#4989 = AXIS2_PLACEMENT_3D ( 'NONE', #7521, #12223, #10242 ) ;
#4990 = CARTESIAN_POINT ( 'NONE',  ( -820.0579670039569464, 81.97422455664136010, -104.6794498541743224 ) ) ;
#4991 = CARTESIAN_POINT ( 'NONE',  ( 87.04832655144112152, 12.00000000000000000, -210.4289243767383368 ) ) ;
#4992 = CARTESIAN_POINT ( 'NONE',  ( -1025.296800000958683, 108.9225844456048691, -146.0307792196446144 ) ) ;
#4993 = CARTESIAN_POINT ( 'NONE',  ( 6.214997436783724833E-15, 139.9999999999999716, -170.4213562373095101 ) ) ;
#4994 = DIRECTION ( 'NONE',  ( -1.000000000000000000, -0.000000000000000000, -0.000000000000000000 ) ) ;
#4995 = ORIENTED_EDGE ( 'NONE', *, *, #8066, .F. ) ;
#4996 = LINE ( 'NONE', #3371, #5694 ) ;
#4997 = CARTESIAN_POINT ( 'NONE',  ( 0.000000000000000000, 164.0000000000000000, -126.4213562373094959 ) ) ;
#4998 = ADVANCED_FACE ( 'NONE', ( #2351 ), #4200, .F. ) ;
#4999 = CARTESIAN_POINT ( 'NONE',  ( 35.00000000000000000, 2.012279232133096230E-14, -124.6807709998040110 ) ) ;
#5000 = CARTESIAN_POINT ( 'NONE',  ( -795.0000000000006821, 98.77454568802552615, -149.7857175106634884 ) ) ;
#5001 = CYLINDRICAL_SURFACE ( 'NONE', #97, 7.500000000000007105 ) ;
#5002 = EDGE_CURVE ( 'NONE', #5830, #8054, #7935, .T. ) ;
#5003 = CARTESIAN_POINT ( 'NONE',  ( -6.097041784444755962E-13, 12.00000000000000000, -237.1807709998039115 ) ) ;
#5004 = EDGE_LOOP ( 'NONE', ( #9906, #7937, #12196, #4108 ) ) ;
#5005 = CARTESIAN_POINT ( 'NONE',  ( -384.6502984881886960, 87.01447873645270192, -144.0511302412744499 ) ) ;
#5006 = CARTESIAN_POINT ( 'NONE',  ( -996.0013826475917540, 63.70094029248592449, -152.5758913445294240 ) ) ;
#5007 = FACE_OUTER_BOUND ( 'NONE', #3643, .T. ) ;
#5008 = CIRCLE ( 'NONE', #7183, 35.00000000000000000 ) ;
#5009 = AXIS2_PLACEMENT_3D ( 'NONE', #2120, #5879, #9658 ) ;
#5010 = DIRECTION ( 'NONE',  ( -8.163404592832030268E-17, 1.000000000000000000, -0.000000000000000000 ) ) ;
#5011 = DIRECTION ( 'NONE',  ( 0.000000000000000000, 0.000000000000000000, 1.000000000000000000 ) ) ;
#5012 = ADVANCED_FACE ( 'NONE', ( #11631 ), #10688, .F. ) ;
#5013 = CIRCLE ( 'NONE', #9757, 7.500000000000007105 ) ;
#5014 = ORIENTED_EDGE ( 'NONE', *, *, #4786, .F. ) ;
#5015 = EDGE_CURVE ( 'NONE', #2820, #9984, #5990, .T. ) ;
#5016 = VECTOR ( 'NONE', #8486, 1000.000000000000000 ) ;
#5017 = CIRCLE ( 'NONE', #11933, 20.00000000000000000 ) ;
#5018 = CARTESIAN_POINT ( 'NONE',  ( -126.4213562373094959, 0.000000000000000000, 2.255140518769849223E-14 ) ) ;
#5019 = EDGE_CURVE ( 'NONE', #7819, #10381, #6343, .T. ) ;
#5020 = CARTESIAN_POINT ( 'NONE',  ( -901.8967518049364571, 57.00804855647901093, -118.7903414690679540 ) ) ;
#5021 = CARTESIAN_POINT ( 'NONE',  ( -19.90044468808352462, 181.3371914423172768, -122.6846776996206358 ) ) ;
#5022 = ORIENTED_EDGE ( 'NONE', *, *, #7195, .T. ) ;
#5023 =( REPRESENTATION_RELATIONSHIP ('NONE','NONE', #12149, #6213 ) REPRESENTATION_RELATIONSHIP_WITH_TRANSFORMATION ( #9731 )SHAPE_REPRESENTATION_RELATIONSHIP( ) );
#5024 = CARTESIAN_POINT ( 'NONE',  ( -372.5472084145004033, 62.44479106828742232, -120.1925590171575351 ) ) ;
#5025 = CARTESIAN_POINT ( 'NONE',  ( -380.2796270122050259, 63.94918908883580144, -116.0487223431423160 ) ) ;
#5026 = DIRECTION ( 'NONE',  ( 0.000000000000000000, 1.000000000000000000, 0.000000000000000000 ) ) ;
#5027 = ORIENTED_EDGE ( 'NONE', *, *, #9627, .F. ) ;
#5028 = ITEM_DEFINED_TRANSFORMATION ( 'NONE', 'NONE', #709,  #11957 ) ;
#5029 = AXIS2_PLACEMENT_3D ( 'NONE', #1386, #4355, #2491 ) ;
#5030 = ORIENTED_EDGE ( 'NONE', *, *, #11602, .F. ) ;
#5031 = CARTESIAN_POINT ( 'NONE',  ( -817.1493800258448346, 27.50875274330015685, -122.7172756069792001 ) ) ;
#5032 = CARTESIAN_POINT ( 'NONE',  ( 1.250503886288004501E-12, 164.0000000000000000, -13.92135623730949057 ) ) ;
#5033 = EDGE_CURVE ( 'NONE', #10254, #8307, #11749, .T. ) ;
#5034 = EDGE_CURVE ( 'NONE', #154, #3651, #11088, .T. ) ;
#5035 = AXIS2_PLACEMENT_3D ( 'NONE', #2346, #10626, #1300 ) ;
#5036 = CARTESIAN_POINT ( 'NONE',  ( -954.7734463792770612, 107.7731650919851205, -99.57582448894495997 ) ) ;
#5037 = CARTESIAN_POINT ( 'NONE',  ( -19.94620750243457863, 178.0808788782996146, -126.1595479531101631 ) ) ;
#5038 = EDGE_LOOP ( 'NONE', ( #1141, #5808 ) ) ;
#5039 = DIRECTION ( 'NONE',  ( -0.000000000000000000, 1.000000000000000000, 7.930164461608263644E-17 ) ) ;
#5040 = ORIENTED_EDGE ( 'NONE', *, *, #2939, .T. ) ;
#5041 = CARTESIAN_POINT ( 'NONE',  ( -794.9999999999997726, 87.89043812168591785, -95.06748246948019698 ) ) ;
#5042 = VERTEX_POINT ( 'NONE', #8037 ) ;
#5043 = CIRCLE ( 'NONE', #5438, 9.000000000000000000 ) ;
#5044 = CARTESIAN_POINT ( 'NONE',  ( -904.1167769183923610, 122.8348148996190758, -136.2353035311977862 ) ) ;
#5045 = CARTESIAN_POINT ( 'NONE',  ( -27.99999999999999645, -6.000000000000000000, 27.99999999999999645 ) ) ;
#5046 = DIRECTION ( 'NONE',  ( 1.000000000000000000, 0.000000000000000000, 0.000000000000000000 ) ) ;
#5047 = CARTESIAN_POINT ( 'NONE',  ( -818.8285638327206470, 78.34153296655567544, -144.3462106687107678 ) ) ;
#5048 = DIRECTION ( 'NONE',  ( 0.000000000000000000, 0.000000000000000000, 1.000000000000000000 ) ) ;
#5049 = FACE_OUTER_BOUND ( 'NONE', #75, .T. ) ;
#5050 = VECTOR ( 'NONE', #10988, 1000.000000000000000 ) ;
#5051 = SURFACE_STYLE_FILL_AREA ( #2394 ) ;
#5052 = FACE_BOUND ( 'NONE', #9824, .T. ) ;
#5053 = EDGE_LOOP ( 'NONE', ( #9764, #3280, #11707 ) ) ;
#5054 = DIRECTION ( 'NONE',  ( 0.000000000000000000, 1.000000000000000000, 0.000000000000000000 ) ) ;
#5055 = FACE_OUTER_BOUND ( 'NONE', #3199, .T. ) ;
#5056 = FACE_OUTER_BOUND ( 'NONE', #5512, .T. ) ;
#5057 = DIRECTION ( 'NONE',  ( 0.000000000000000000, 1.000000000000000000, 0.000000000000000000 ) ) ;
#5058 = CARTESIAN_POINT ( 'NONE',  ( -1022.396981161619806, 109.5926079579672603, -146.0307792196444154 ) ) ;
#5059 = LINE ( 'NONE', #7104, #9328 ) ;
#5060 = ORIENTED_EDGE ( 'NONE', *, *, #504, .T. ) ;
#5061 = AXIS2_PLACEMENT_3D ( 'NONE', #11224, #5586, #1825 ) ;
#5062 = ORIENTED_EDGE ( 'NONE', *, *, #1884, .T. ) ;
#5063 = EDGE_CURVE ( 'NONE', #9727, #9411, #8902, .T. ) ;
#5064 = FACE_BOUND ( 'NONE', #4920, .T. ) ;
#5065 = CARTESIAN_POINT ( 'NONE',  ( -795.0000000000071623, 70.44548139156209743, -152.5758913445292535 ) ) ;
#5066 = DIRECTION ( 'NONE',  ( 1.000000000000000000, 0.000000000000000000, -0.000000000000000000 ) ) ;
#5067 = CARTESIAN_POINT ( 'NONE',  ( 0.000000000000000000, 0.000000000000000000, 0.000000000000000000 ) ) ;
#5068 = VECTOR ( 'NONE', #9063, 1000.000000000000000 ) ;
#5069 = DIRECTION ( 'NONE',  ( 0.000000000000000000, 1.000000000000000000, 0.000000000000000000 ) ) ;
#5070 = CARTESIAN_POINT ( 'NONE',  ( 56.53599999999998715, 7.347880794884118750E-16, -5.999999999999999112 ) ) ;
#5071 = AXIS2_PLACEMENT_3D ( 'NONE', #11029, #10100, #1828 ) ;
#5072 = LINE ( 'NONE', #5881, #6076 ) ;
#5073 = ORIENTED_EDGE ( 'NONE', *, *, #3720, .F. ) ;
#5074 = AXIS2_PLACEMENT_3D ( 'NONE', #3450, #4048, #10068 ) ;
#5075 = ORIENTED_EDGE ( 'NONE', *, *, #340, .F. ) ;
#5076 = ORIENTED_EDGE ( 'NONE', *, *, #3203, .F. ) ;
#5077 = LINE ( 'NONE', #429, #4080 ) ;
#5078 = PRESENTATION_LAYER_ASSIGNMENT (  '', '', ( #1159 ) ) ;
#5079 = ADVANCED_FACE ( 'NONE', ( #539 ), #4379, .T. ) ;
#5080 = CARTESIAN_POINT ( 'NONE',  ( -1057.805062346511704, 42.77845103615958067, -118.7903414690684087 ) ) ;
#5081 = CYLINDRICAL_SURFACE ( 'NONE', #7254, 7.500000000000007105 ) ;
#5082 = EDGE_CURVE ( 'NONE', #11519, #9164, #6152, .T. ) ;
#5083 = ORIENTED_EDGE ( 'NONE', *, *, #12205, .F. ) ;
#5084 = CARTESIAN_POINT ( 'NONE',  ( -818.9871366297778650, 79.96561131121026733, -144.5796535119517614 ) ) ;
#5085 = CARTESIAN_POINT ( 'NONE',  ( -370.4431240880659288, 57.15653990294408970, -114.9924028572851142 ) ) ;
#5086 = CARTESIAN_POINT ( 'NONE',  ( 7.500000000000000000, 0.000000000000000000, 8.999999999999998224 ) ) ;
#5087 = EDGE_LOOP ( 'NONE', ( #1151, #8768, #7958, #304 ) ) ;
#5088 = DIRECTION ( 'NONE',  ( 0.000000000000000000, 0.000000000000000000, 1.000000000000000000 ) ) ;
#5089 = ORIENTED_EDGE ( 'NONE', *, *, #3485, .F. ) ;
#5090 = EDGE_LOOP ( 'NONE', ( #2013, #9970 ) ) ;
#5091 = CARTESIAN_POINT ( 'NONE',  ( -817.4144546772188278, 30.82543593413045713, -113.1262384684093689 ) ) ;
#5092 = CONICAL_SURFACE ( 'NONE', #10826, 5.035999999999999588, 0.7853981633974410625 ) ;
#5093 = EDGE_CURVE ( 'NONE', #9388, #2064, #2460, .T. ) ;
#5094 = DIRECTION ( 'NONE',  ( 0.000000000000000000, 1.000000000000000000, 0.000000000000000000 ) ) ;
#5095 = UNCERTAINTY_MEASURE_WITH_UNIT (LENGTH_MEASURE( 1.000000000000000082E-05 ), #5744, 'distance_accuracy_value', 'NONE');
#5096 = VECTOR ( 'NONE', #11348, 1000.000000000000000 ) ;
#5097 = CARTESIAN_POINT ( 'NONE',  ( -1018.401127491270358, 110.2021201405460431, -103.3307627799636208 ) ) ;
#5098 = DIRECTION ( 'NONE',  ( 0.000000000000000000, 0.000000000000000000, -1.000000000000000000 ) ) ;
#5099 = CARTESIAN_POINT ( 'NONE',  ( 45.53315400109643463, 12.00000000000000000, -237.8419396193597208 ) ) ;
#5100 = CARTESIAN_POINT ( 'NONE',  ( -374.4497035394655882, 90.81972200502131898, -96.39717024633597475 ) ) ;
#5101 = AXIS2_PLACEMENT_3D ( 'NONE', #11005, #6309, #883 ) ;
#5102 = VERTEX_POINT ( 'NONE', #8152 ) ;
#5103 = CARTESIAN_POINT ( 'NONE',  ( -374.9131056416630940, 86.31065638273830132, -105.1272594036523458 ) ) ;
#5104 = EDGE_CURVE ( 'NONE', #8436, #11949, #5357, .T. ) ;
#5105 = ORIENTED_EDGE ( 'NONE', *, *, #1847, .F. ) ;
#5106 = CARTESIAN_POINT ( 'NONE',  ( -1061.884876827091830, 80.20192378191423188, -94.48732055948617869 ) ) ;
#5107 = DIRECTION ( 'NONE',  ( -0.9501779778103313090, 0.000000000000000000, -0.3117078928809301486 ) ) ;
#5108 = AXIS2_PLACEMENT_3D ( 'NONE', #4759, #2217, #6912 ) ;
#5109 = CARTESIAN_POINT ( 'NONE',  ( -1017.810720698609543, 119.7719591276204625, -124.6807709998040679 ) ) ;
#5110 = DIRECTION ( 'NONE',  ( 0.000000000000000000, -0.8660254037844380415, -0.5000000000000009992 ) ) ;
#5111 = EDGE_CURVE ( 'NONE', #10867, #11480, #1477, .T. ) ;
#5112 = DIRECTION ( 'NONE',  ( -0.000000000000000000, 1.189524669241239115E-16, -1.000000000000000000 ) ) ;
#5113 = VECTOR ( 'NONE', #2719, 1000.000000000000000 ) ;
#5114 = CARTESIAN_POINT ( 'NONE',  ( -1031.000617048998265, 115.3267894020684992, -113.1262384684098521 ) ) ;
#5115 = DIRECTION ( 'NONE',  ( 0.000000000000000000, 0.000000000000000000, -1.000000000000000000 ) ) ;
#5116 = CIRCLE ( 'NONE', #5515, 44.00000000000001421 ) ;
#5117 = B_SPLINE_CURVE_WITH_KNOTS ( 'NONE', 3,
 ( #1549, #8847, #3162, #6188, #2239, #9082, #6251, #7112, #374, #11700, #10018, #6066, #10876, #8896, #4099, #557, #11870, #5311, #3213, #2411, #1370, #2361, #9959, #7870, #6007, #5248, #4212, #1315, #6128, #9895, #4337, #3644, #5506, #4460, #3455, #2595 ),
 .UNSPECIFIED., .F., .F.,
 ( 4, 2, 2, 2, 2, 2, 2, 2, 2, 2, 2, 2, 2, 2, 2, 2, 2, 4 ),
 ( 0.01566740727309163389, 0.01664433654934411103, 0.01762126582559659163, 0.01859819510184906877, 0.01957512437810154590, 0.02055205365435402304, 0.02152898293060650364, 0.02250591220685898078, 0.02348284148311145791, 0.02445977075936393852, 0.02494823539749017882, 0.02543670003561641565, 0.02641362931186860483, 0.02739055858812079053, 0.02836748786437297970, 0.02934441714062516887, 0.03032134641687735804, 0.03129827569312954721 ),
 .UNSPECIFIED. ) ;
#5118 = STYLED_ITEM ( 'NONE', ( #1237 ), #3982 ) ;
#5119 = CARTESIAN_POINT ( 'NONE',  ( -827.6025323198946353, 81.97067649012244317, -104.6794282814518624 ) ) ;
#5120 = DIRECTION ( 'NONE',  ( -0.000000000000000000, 1.000000000000000000, 7.930164461608263644E-17 ) ) ;
#5121 = CIRCLE ( 'NONE', #6296, 20.00000000000008882 ) ;
#5122 = EDGE_CURVE ( 'NONE', #6181, #11388, #10003, .T. ) ;
#5123 = CARTESIAN_POINT ( 'NONE',  ( -823.8285638327206470, 78.67432280806529832, -264.6807709998040536 ) ) ;
#5124 = DIRECTION ( 'NONE',  ( -0.000000000000000000, -1.000000000000000000, 0.000000000000000000 ) ) ;
#5125 = ORIENTED_EDGE ( 'NONE', *, *, #11852, .F. ) ;
#5126 = CARTESIAN_POINT ( 'NONE',  ( 120.8820948793965186, 12.00000000000000000, -186.6989091883332890 ) ) ;
#5127 = CARTESIAN_POINT ( 'NONE',  ( -1030.931480980267906, 117.9615145441170654, -124.6807709998043521 ) ) ;
#5128 = DIRECTION ( 'NONE',  ( 0.000000000000000000, 0.000000000000000000, 1.000000000000000000 ) ) ;
#5129 = CARTESIAN_POINT ( 'NONE',  ( 2.498657532616778856E-14, -6.999999999999978684, -124.6807709998038405 ) ) ;
#5130 = EDGE_LOOP ( 'NONE', ( #12006, #6852, #5386, #10778 ) ) ;
#5131 = CARTESIAN_POINT ( 'NONE',  ( -379.6799153206045503, 62.87498284247939040, -130.5615721467151786 ) ) ;
#5132 = DIRECTION ( 'NONE',  ( 0.000000000000000000, 0.000000000000000000, 1.000000000000000000 ) ) ;
#5133 = DIRECTION ( 'NONE',  ( -0.000000000000000000, 1.000000000000000000, 7.930164461608263644E-17 ) ) ;
#5134 = DIRECTION ( 'NONE',  ( -1.000000000000000000, 0.000000000000000000, 0.000000000000000000 ) ) ;
#5135 = CARTESIAN_POINT ( 'NONE',  ( 87.04832655144112152, 12.00000000000000000, -217.9289243767383368 ) ) ;
#5136 = SURFACE_STYLE_FILL_AREA ( #6008 ) ;
#5137 = ORIENTED_EDGE ( 'NONE', *, *, #414, .T. ) ;
#5138 = CARTESIAN_POINT ( 'NONE',  ( -1027.708477481189902, 65.70736702952426356, -149.7857175106639431 ) ) ;
#5139 = ORIENTED_EDGE ( 'NONE', *, *, #11277, .T. ) ;
#5140 = ORIENTED_EDGE ( 'NONE', *, *, #165, .F. ) ;
#5141 = CARTESIAN_POINT ( 'NONE',  ( 19.97976963877082923, 177.9666655783959186, -123.7712089892055189 ) ) ;
#5142 = CARTESIAN_POINT ( 'NONE',  ( -1064.999999999999545, 54.10491585757062438, -113.1262384684097668 ) ) ;
#5143 = ORIENTED_EDGE ( 'NONE', *, *, #9340, .F. ) ;
#5144 = CARTESIAN_POINT ( 'NONE',  ( -824.4843289719594850, 83.64195140549487917, -95.25604041866178306 ) ) ;
#5145 = VERTEX_POINT ( 'NONE', #10123 ) ;
#5146 = VERTEX_POINT ( 'NONE', #3498 ) ;
#5147 = TOROIDAL_SURFACE ( 'NONE', #8121, 10.00000000000003730, 1.499999999999998002 ) ;
#5148 = ORIENTED_EDGE ( 'NONE', *, *, #2970, .F. ) ;
#5149 = EDGE_CURVE ( 'NONE', #3632, #3075, #11096, .T. ) ;
#5150 = CARTESIAN_POINT ( 'NONE',  ( -172.5000000000000000, 139.9999999999999716, -126.4213562373082453 ) ) ;
#5151 = ADVANCED_FACE ( 'NONE', ( #4446 ), #9130, .F. ) ;
#5152 = DIRECTION ( 'NONE',  ( -8.163404592832031500E-17, 1.000000000000000000, 0.000000000000000000 ) ) ;
#5153 = CARTESIAN_POINT ( 'NONE',  ( -955.0423082396529253, 101.0797422464698059, -96.78565065507901011 ) ) ;
#5154 = LINE ( 'NONE', #444, #11398 ) ;
#5155 = DIRECTION ( 'NONE',  ( 2.040851148208007875E-17, -1.000000000000000000, -0.000000000000000000 ) ) ;
#5156 = ADVANCED_FACE ( 'NONE', ( #4508 ), #6237, .F. ) ;
#5157 = ORIENTED_EDGE ( 'NONE', *, *, #807, .F. ) ;
#5158 = CYLINDRICAL_SURFACE ( 'NONE', #8168, 7.500000000000007105 ) ;
#5159 = DIRECTION ( 'NONE',  ( 3.061276722312011504E-17, -1.000000000000000000, -0.000000000000000000 ) ) ;
#5160 = VECTOR ( 'NONE', #4561, 1000.000000000000000 ) ;
#5161 = ORIENTED_EDGE ( 'NONE', *, *, #4119, .F. ) ;
#5162 = DIRECTION ( 'NONE',  ( 0.000000000000000000, 0.000000000000000000, -1.000000000000000000 ) ) ;
#5163 = VERTEX_POINT ( 'NONE', #2711 ) ;
#5164 = CARTESIAN_POINT ( 'NONE',  ( -1026.284439350007460, 91.37828661775220951, -95.06748246948018277 ) ) ;
#5165 = DIRECTION ( 'NONE',  ( -1.000000000000000000, 0.000000000000000000, 0.000000000000000000 ) ) ;
#5166 = CARTESIAN_POINT ( 'NONE',  ( -1037.337636019038882, 116.9882293220588991, -124.6807709998043521 ) ) ;
#5167 = CARTESIAN_POINT ( 'NONE',  ( 141.4213562373095101, -6.000000000000000000, -1.508194112741312283E-14 ) ) ;
#5168 = CIRCLE ( 'NONE', #4382, 7.500000000000005329 ) ;
#5169 = EDGE_CURVE ( 'NONE', #10118, #931, #8911, .T. ) ;
#5170 = ORIENTED_EDGE ( 'NONE', *, *, #2317, .T. ) ;
#5171 = CARTESIAN_POINT ( 'NONE',  ( -19.93086114385802077, 181.8378500852114712, -123.0137796683760456 ) ) ;
#5172 = CARTESIAN_POINT ( 'NONE',  ( -828.7652305532230912, 79.48420453549654496, -104.8389787515929754 ) ) ;
#5173 = CARTESIAN_POINT ( 'NONE',  ( -1025.976186494711783, 52.68972726728017619, -124.6807709998042952 ) ) ;
#5174 = CARTESIAN_POINT ( 'NONE',  ( -820.7733255381026538, 82.64589962596730288, -95.09174178707476699 ) ) ;
#5175 = DIRECTION ( 'NONE',  ( 1.000000000000000000, 0.000000000000000000, 0.000000000000000000 ) ) ;
#5176 = EDGE_LOOP ( 'NONE', ( #25, #12049, #8796, #6763 ) ) ;
#5177 = DIRECTION ( 'NONE',  ( 0.000000000000000000, 1.000000000000000000, 0.000000000000000000 ) ) ;
#5178 = CIRCLE ( 'NONE', #11301, 1.000000000000000888 ) ;
#5179 = CARTESIAN_POINT ( 'NONE',  ( -1017.810720698609543, 119.7719591276204625, -124.6807709998040679 ) ) ;
#5180 = FACE_OUTER_BOUND ( 'NONE', #6618, .T. ) ;
#5181 = DIRECTION ( 'NONE',  ( 0.000000000000000000, 1.000000000000000000, 0.000000000000000000 ) ) ;
#5182 = DIRECTION ( 'NONE',  ( 0.000000000000000000, -1.000000000000000000, 0.000000000000000000 ) ) ;
#5183 = VERTEX_POINT ( 'NONE', #2641 ) ;
#5184 = EDGE_CURVE ( 'NONE', #4714, #1702, #6560, .T. ) ;
#5185 = ORIENTED_EDGE ( 'NONE', *, *, #7991, .F. ) ;
#5186 = CARTESIAN_POINT ( 'NONE',  ( -384.9888944676742426, 83.49078106762718221, -144.6610261000669198 ) ) ;
#5187 = DIRECTION ( 'NONE',  ( 1.000000000000000000, 0.000000000000000000, 0.000000000000000000 ) ) ;
#5188 = DIRECTION ( 'NONE',  ( -8.163404592832030268E-17, 1.000000000000000000, -0.000000000000000000 ) ) ;
#5189 = LINE ( 'NONE', #6935, #10639 ) ;
#5190 = AXIS2_PLACEMENT_3D ( 'NONE', #8404, #4495, #921 ) ;
#5191 = VERTEX_POINT ( 'NONE', #3441 ) ;
#5192 = CARTESIAN_POINT ( 'NONE',  ( -902.2382941300837729, 66.55116351576596401, -146.0307792196448986 ) ) ;
#5193 = VERTEX_POINT ( 'NONE', #4576 ) ;
#5194 = AXIS2_PLACEMENT_3D ( 'NONE', #6670, #4012, #7780 ) ;
#5195 = VECTOR ( 'NONE', #7622, 1000.000000000000000 ) ;
#5196 = CARTESIAN_POINT ( 'NONE',  ( -997.9925905826713688, 37.72784750336357007, -118.7903414690684514 ) ) ;
#5197 = ORIENTED_EDGE ( 'NONE', *, *, #9793, .F. ) ;
#5198 = CARTESIAN_POINT ( 'NONE',  ( 9.371890508914830252E-13, 152.0000000000000000, -36.42135623730948168 ) ) ;
#5199 = ORIENTED_EDGE ( 'NONE', *, *, #3118, .T. ) ;
#5200 = ORIENTED_EDGE ( 'NONE', *, *, #3181, .F. ) ;
#5201 = VECTOR ( 'NONE', #2632, 1000.000000000000000 ) ;
#5202 = CIRCLE ( 'NONE', #12141, 7.500000000000008882 ) ;
#5203 = AXIS2_PLACEMENT_3D ( 'NONE', #5766, #2878, #5891 ) ;
#5204 = CARTESIAN_POINT ( 'NONE',  ( -21.06521297978533980, 179.6586675211645741, -126.3290294770899891 ) ) ;
#5205 = CARTESIAN_POINT ( 'NONE',  ( -1065.000000000008868, 103.3499740386314016, -103.3307627799635924 ) ) ;
#5206 = FACE_OUTER_BOUND ( 'NONE', #9640, .T. ) ;
#5207 = ADVANCED_FACE ( 'NONE', ( #7224 ), #2517, .F. ) ;
#5208 = AXIS2_PLACEMENT_3D ( 'NONE', #9113, #2691, #11033 ) ;
#5209 = EDGE_LOOP ( 'NONE', ( #11807, #217 ) ) ;
#5210 = AXIS2_PLACEMENT_3D ( 'NONE', #1962, #10125, #6294 ) ;
#5211 = DIRECTION ( 'NONE',  ( -1.000000000000000000, -1.186840563529527301E-16, 0.000000000000000000 ) ) ;
#5212 = CYLINDRICAL_SURFACE ( 'NONE', #10574, 45.00000000000000711 ) ;
#5213 = CARTESIAN_POINT ( 'NONE',  ( -384.8563257790743251, 85.26078067811664596, -104.9374514401265515 ) ) ;
#5214 = VERTEX_POINT ( 'NONE', #12045 ) ;
#5215 = CARTESIAN_POINT ( 'NONE',  ( 9.371890508914830252E-13, 0.000000000000000000, -36.42135623730949590 ) ) ;
#5216 = CARTESIAN_POINT ( 'NONE',  ( -795.0000000000047748, 112.0000000000007532, -124.6807709998042384 ) ) ;
#5217 = EDGE_LOOP ( 'NONE', ( #5959, #5712 ) ) ;
#5218 = FACE_OUTER_BOUND ( 'NONE', #2501, .T. ) ;
#5219 = CARTESIAN_POINT ( 'NONE',  ( -1016.123300349496276, 74.17810748283143596, -96.78565065507957854 ) ) ;
#5220 = DIRECTION ( 'NONE',  ( -1.000000000000000000, -0.000000000000000000, -0.000000000000000000 ) ) ;
#5221 = CARTESIAN_POINT ( 'NONE',  ( -926.5138833012656505, 125.7648744980332225, -126.6442663926294330 ) ) ;
#5222 = CARTESIAN_POINT ( 'NONE',  ( 21.06320946107762282, 180.4881934621326991, -126.4026505290603808 ) ) ;
#5223 = AXIS2_PLACEMENT_3D ( 'NONE', #838, #6636, #10468 ) ;
#5224 = DIRECTION ( 'NONE',  ( -0.000000000000000000, 1.000000000000000000, 7.930164461608263644E-17 ) ) ;
#5225 = AXIS2_PLACEMENT_3D ( 'NONE', #520, #10972, #8133 ) ;
#5226 = CARTESIAN_POINT ( 'NONE',  ( -925.0000000000000000, 81.99999999999988631, -124.6807709998038405 ) ) ;
#5227 = FACE_BOUND ( 'NONE', #9610, .T. ) ;
#5228 = CARTESIAN_POINT ( 'NONE',  ( -954.5692209181579528, 49.02792041507773746, -124.6807709998042384 ) ) ;
#5229 = EDGE_CURVE ( 'NONE', #1988, #10372, #10698, .T. ) ;
#5230 = CARTESIAN_POINT ( 'NONE',  ( -821.3191871189538915, 83.01147993754599952, -95.14350462154642685 ) ) ;
#5231 =( GEOMETRIC_REPRESENTATION_CONTEXT ( 3 ) GLOBAL_UNCERTAINTY_ASSIGNED_CONTEXT ( ( #6835 ) ) GLOBAL_UNIT_ASSIGNED_CONTEXT ( ( #7077, #7202, #5973 ) ) REPRESENTATION_CONTEXT ( 'NONE', 'WORKASPACE' ) );
#5232 = VERTEX_POINT ( 'NONE', #1730 ) ;
#5233 = FACE_OUTER_BOUND ( 'NONE', #6829, .T. ) ;
#5234 = CARTESIAN_POINT ( 'NONE',  ( -852.8175266017511831, 121.6828083272127685, -124.6807709998041247 ) ) ;
#5235 = DIRECTION ( 'NONE',  ( -1.000000000000000000, 0.000000000000000000, 0.000000000000000000 ) ) ;
#5236 = DIRECTION ( 'NONE',  ( 0.000000000000000000, -1.156482317317870246E-16, 1.000000000000000000 ) ) ;
#5237 = DIRECTION ( 'NONE',  ( -1.000000000000000000, -1.156482317317870492E-16, 0.000000000000000000 ) ) ;
#5238 = CARTESIAN_POINT ( 'NONE',  ( -993.6119331254993767, 96.30709745136249467, -152.5758913445288840 ) ) ;
#5239 = ORIENTED_EDGE ( 'NONE', *, *, #11550, .T. ) ;
#5240 = CARTESIAN_POINT ( 'NONE',  ( 19.95910083177870220, 180.2168005683687113, -123.1884788074740271 ) ) ;
#5241 = AXIS2_PLACEMENT_3D ( 'NONE', #8286, #5352, #8219 ) ;
#5242 = DIRECTION ( 'NONE',  ( -0.000000000000000000, 1.000000000000000000, -0.000000000000000000 ) ) ;
#5243 = DIRECTION ( 'NONE',  ( 0.000000000000000000, -1.000000000000000000, -7.930164461608263644E-17 ) ) ;
#5244 = CARTESIAN_POINT ( 'NONE',  ( -370.4401466759219375, 106.8513018378076964, -134.3428354745942102 ) ) ;
#5245 = DIRECTION ( 'NONE',  ( -0.000000000000000000, 1.000000000000000000, -0.000000000000000000 ) ) ;
#5246 = CARTESIAN_POINT ( 'NONE',  ( -381.3731125161232285, 66.09867141544387437, -112.4817134149344184 ) ) ;
#5247 = EDGE_CURVE ( 'NONE', #5440, #11672, #10908, .T. ) ;
#5248 = CARTESIAN_POINT ( 'NONE',  ( -820.7839104893611193, 74.69477923707955824, -94.69500076520461107 ) ) ;
#5250 = ADVANCED_FACE ( 'NONE', ( #8065 ), #4232, .T. ) ;
#5249 = FACE_OUTER_BOUND ( 'NONE', #8605, .T. ) ;
#5251 = ORIENTED_EDGE ( 'NONE', *, *, #12036, .T. ) ;
#5252 = CARTESIAN_POINT ( 'NONE',  ( -795.0000000000039790, 54.10491585757074517, -136.2353035311982410 ) ) ;
#5253 = AXIS2_PLACEMENT_3D ( 'NONE', #986, #2900, #1678 ) ;
#5254 = ORIENTED_EDGE ( 'NONE', *, *, #5002, .T. ) ;
#5255 = ADVANCED_FACE ( 'NONE', ( #3471 ), #32, .T. ) ;
#5256 = EDGE_CURVE ( 'NONE', #1493, #11133, #10212, .T. ) ;
#5257 = ORIENTED_EDGE ( 'NONE', *, *, #11914, .F. ) ;
#5258 = CARTESIAN_POINT ( 'NONE',  ( -172.5000000000000000, 24.00000000000001421, -126.4213562373082453 ) ) ;
#5259 = CARTESIAN_POINT ( 'NONE',  ( -19.86581666024647319, 179.0285536720372477, -126.9951615115761143 ) ) ;
#5260 = AXIS2_PLACEMENT_3D ( 'NONE', #66, #9414, #3845 ) ;
#5261 = DIRECTION ( 'NONE',  ( 0.000000000000000000, 0.000000000000000000, -1.000000000000000000 ) ) ;
#5262 = DIRECTION ( 'NONE',  ( 0.000000000000000000, 0.4999999999999995004, -0.8660254037844389297 ) ) ;
#5263 = EDGE_LOOP ( 'NONE', ( #7118, #1286 ) ) ;
#5265 = EDGE_CURVE ( 'NONE', #6610, #5632, #598, .T. ) ;
#5264 = FACE_OUTER_BOUND ( 'NONE', #8950, .T. ) ;
#5266 = CARTESIAN_POINT ( 'NONE',  ( -21.06656016739612269, 179.5324992879768899, -126.2719758226758273 ) ) ;
#5267 = AXIS2_PLACEMENT_3D ( 'NONE', #2221, #9756, #1302 ) ;
#5268 = AXIS2_PLACEMENT_3D ( 'NONE', #6576, #5703, #12148 ) ;
#5269 = DIRECTION ( 'NONE',  ( 1.000000000000000000, -1.026341648675396322E-47, 2.081668171172161734E-17 ) ) ;
#5270 = CARTESIAN_POINT ( 'NONE',  ( -794.9999999999997726, 87.89043812168591785, -95.06748246948019698 ) ) ;
#5271 = CARTESIAN_POINT ( 'NONE',  ( -30.00000000000000000, -492.9999999999998863, -30.00000000000000000 ) ) ;
#5272 = ORIENTED_EDGE ( 'NONE', *, *, #3976, .F. ) ;
#5273 = CARTESIAN_POINT ( 'NONE',  ( -374.8169097728642214, 87.13039421098122261, -95.24255214225362920 ) ) ;
#5274 = ORIENTED_EDGE ( 'NONE', *, *, #7230, .F. ) ;
#5275 = AXIS2_PLACEMENT_3D ( 'NONE', #2580, #3442, #10930 ) ;
#5276 = DIRECTION ( 'NONE',  ( 0.000000000000000000, 1.000000000000000000, 0.000000000000000000 ) ) ;
#5277 = DIRECTION ( 'NONE',  ( 0.000000000000000000, 1.000000000000000000, 0.000000000000000000 ) ) ;
#5278 = ORIENTED_EDGE ( 'NONE', *, *, #10098, .F. ) ;
#5279 = CARTESIAN_POINT ( 'NONE',  ( -827.1386055644237558, 82.43593308702942579, -154.2518061096776876 ) ) ;
#5280 = CARTESIAN_POINT ( 'NONE',  ( -853.4539021257702416, 72.48584973915980356, -94.48732055948642028 ) ) ;
#5281 = CARTESIAN_POINT ( 'NONE',  ( -14.74749198504467174, 180.2041921146325478, -184.6327933705055386 ) ) ;
#5282 = CARTESIAN_POINT ( 'NONE',  ( -21.06240745282767080, 180.2041921146517041, -126.4269926335259413 ) ) ;
#5283 = VECTOR ( 'NONE', #10241, 1000.000000000000000 ) ;
#5284 = VECTOR ( 'NONE', #11190, 1000.000000000000000 ) ;
#5285 = CARTESIAN_POINT ( 'NONE',  ( 0.000000000000000000, 0.000000000000000000, 0.000000000000000000 ) ) ;
#5286 = CARTESIAN_POINT ( 'NONE',  ( -819.8405841167650578, 75.64117232352664644, -143.6450765909189329 ) ) ;
#5287 = CARTESIAN_POINT ( 'NONE',  ( 3.123963502971610252E-13, -6.000000000000006217, -88.92135623730948168 ) ) ;
#5288 = CARTESIAN_POINT ( 'NONE',  ( -1038.719578313838156, 40.52245044769760085, -124.6807709998045652 ) ) ;
#5289 = PLANE ( 'NONE',  #9372 ) ;
#5290 = ORIENTED_EDGE ( 'NONE', *, *, #11375, .F. ) ;
#5291 = CARTESIAN_POINT ( 'NONE',  ( -954.0441199534440102, 124.9954171138387977, -124.6807709998039115 ) ) ;
#5292 = AXIS2_PLACEMENT_3D ( 'NONE', #9626, #159, #221 ) ;
#5293 = CARTESIAN_POINT ( 'NONE',  ( 3.123963502971610252E-13, 152.0000000000000000, -96.42135623730948168 ) ) ;
#5294 = DIRECTION ( 'NONE',  ( 0.000000000000000000, 0.000000000000000000, -1.000000000000000000 ) ) ;
#5295 = CARTESIAN_POINT ( 'NONE',  ( -370.4431240880636551, 57.15653990293812825, -114.9924028573050663 ) ) ;
#5296 = EDGE_CURVE ( 'NONE', #2780, #8550, #7526, .T. ) ;
#5297 = FACE_OUTER_BOUND ( 'NONE', #10656, .T. ) ;
#5298 = ADVANCED_FACE ( 'NONE', ( #3837 ), #2046, .F. ) ;
#5299 = VERTEX_POINT ( 'NONE', #9587 ) ;
#5300 = STYLED_ITEM ( 'NONE', ( #8594 ), #3942 ) ;
#5301 = VECTOR ( 'NONE', #3311, 1000.000000000000000 ) ;
#5302 = ORIENTED_EDGE ( 'NONE', *, *, #1692, .F. ) ;
#5303 = CARTESIAN_POINT ( 'NONE',  ( -19.99667327426407937, 177.7725865070964062, -124.2645694134507153 ) ) ;
#5304 = DIRECTION ( 'NONE',  ( -0.000000000000000000, 1.000000000000000000, 0.000000000000000000 ) ) ;
#5305 = CARTESIAN_POINT ( 'NONE',  ( -953.2897746444480163, 79.65961628290892804, -154.2940595301281519 ) ) ;
#5306 = DIRECTION ( 'NONE',  ( -8.163404592832030268E-17, 1.000000000000000000, -0.000000000000000000 ) ) ;
#5307 = ADVANCED_FACE ( 'NONE', ( #2860 ), #8543, .F. ) ;
#5308 = CARTESIAN_POINT ( 'NONE',  ( 0.07661102881317116697, -8.673996836102535468, 2.976196775178697518 ) ) ;
#5309 = CARTESIAN_POINT ( 'NONE',  ( -955.0000000000038654, 82.00000000000036948, -124.6807709998041673 ) ) ;
#5310 = DIRECTION ( 'NONE',  ( 0.000000000000000000, 0.000000000000000000, 1.000000000000000000 ) ) ;
#5311 = CARTESIAN_POINT ( 'NONE',  ( -823.5029313004960159, 73.67403370300826282, -94.71553284777590420 ) ) ;
#5312 = CARTESIAN_POINT ( 'NONE',  ( 2.187692937179487324E-12, -6.000000000000004441, 76.07864376269048989 ) ) ;
#5313 = AXIS2_PLACEMENT_3D ( 'NONE', #11291, #5779, #9618 ) ;
#5314 = DIRECTION ( 'NONE',  ( 0.000000000000000000, 0.000000000000000000, -1.000000000000000000 ) ) ;
#5315 = VERTEX_POINT ( 'NONE', #1990 ) ;
#5316 = CARTESIAN_POINT ( 'NONE',  ( -1048.040919118598822, 50.77060569800413248, -146.0307792196448986 ) ) ;
#5317 = ORIENTED_EDGE ( 'NONE', *, *, #7462, .F. ) ;
#5318 = ORIENTED_EDGE ( 'NONE', *, *, #10551, .T. ) ;
#5319 = EDGE_CURVE ( 'NONE', #6347, #10683, #1245, .T. ) ;
#5320 = LINE ( 'NONE', #9965, #5588 ) ;
#5321 = DIRECTION ( 'NONE',  ( 0.000000000000000000, 1.689469820081758265E-14, -1.000000000000000000 ) ) ;
#5322 = FACE_BOUND ( 'NONE', #5801, .T. ) ;
#5323 = VERTEX_POINT ( 'NONE', #3030 ) ;
#5324 = CARTESIAN_POINT ( 'NONE',  ( -379.2145310736904662, 62.08676270979725587, -126.6546628987567402 ) ) ;
#5325 = CARTESIAN_POINT ( 'NONE',  ( -381.3375926232646975, 97.95623339593267076, -112.6086769336026663 ) ) ;
#5326 = ORIENTED_EDGE ( 'NONE', *, *, #1619, .T. ) ;
#5327 = ADVANCED_FACE ( 'NONE', ( #7670 ), #5748, .F. ) ;
#5328 = PLANE ( 'NONE',  #5675 ) ;
#5329 = ORIENTED_EDGE ( 'NONE', *, *, #12228, .F. ) ;
#5330 = CARTESIAN_POINT ( 'NONE',  ( 6.899999999999999467, -10.39230484541326405, 0.000000000000000000 ) ) ;
#5331 = CARTESIAN_POINT ( 'NONE',  ( 19.00000000000000355, 167.0000000000000000, -124.6807709998038405 ) ) ;
#5332 = EDGE_CURVE ( 'NONE', #2055, #8525, #3776, .T. ) ;
#5333 = CARTESIAN_POINT ( 'NONE',  ( -1062.096538105501168, 73.81465972843167833, -95.06748246948046699 ) ) ;
#5334 = DIRECTION ( 'NONE',  ( 0.000000000000000000, 0.000000000000000000, 1.000000000000000000 ) ) ;
#5335 = CARTESIAN_POINT ( 'NONE',  ( 141.4213562373095101, -492.9999999999998863, -1.508194112741312283E-14 ) ) ;
#5336 = ORIENTED_EDGE ( 'NONE', *, *, #6679, .F. ) ;
#5337 = DIRECTION ( 'NONE',  ( 0.000000000000000000, -1.156482317317870246E-16, 1.000000000000000000 ) ) ;
#5338 = FACE_OUTER_BOUND ( 'NONE', #6011, .T. ) ;
#5339 = DIRECTION ( 'NONE',  ( 0.000000000000000000, 1.000000000000000000, 0.000000000000000000 ) ) ;
#5340 = EDGE_LOOP ( 'NONE', ( #7561, #802 ) ) ;
#5341 = LINE ( 'NONE', #8923, #945 ) ;
#5342 = CARTESIAN_POINT ( 'NONE',  ( -1065.000000000001364, 70.44548139156162847, -96.78565065507940801 ) ) ;
#5343 = FACE_OUTER_BOUND ( 'NONE', #1785, .T. ) ;
#5344 = CARTESIAN_POINT ( 'NONE',  ( -379.7887390581964837, 100.9343252097582564, -131.1221473163307678 ) ) ;
#5345 = CARTESIAN_POINT ( 'NONE',  ( 1.561981751485805177E-12, -6.000000000000005329, 23.57864376269050410 ) ) ;
#5346 = CARTESIAN_POINT ( 'NONE',  ( -823.1660337641022807, 73.70728137675511960, -106.4808805636500324 ) ) ;
#5347 = CARTESIAN_POINT ( 'NONE',  ( -828.1715959468207302, 76.17590192436144036, -143.8160639703673098 ) ) ;
#5348 = CARTESIAN_POINT ( 'NONE',  ( -825.4402961394276872, 83.41886444745699691, -104.7307635270714314 ) ) ;
#5349 = LINE ( 'NONE', #9125, #7565 ) ;
#5350 = CARTESIAN_POINT ( 'NONE',  ( -819.4886076266410555, 76.16999570164527711, -154.6813788771335680 ) ) ;
#5351 = ORIENTED_EDGE ( 'NONE', *, *, #10852, .F. ) ;
#5352 = DIRECTION ( 'NONE',  ( -1.224646799147353207E-16, -3.748982739283705415E-33, 1.000000000000000000 ) ) ;
#5353 = CARTESIAN_POINT ( 'NONE',  ( -1030.944970944895431, 117.4714819019837222, -118.7903414690680535 ) ) ;
#5354 = CARTESIAN_POINT ( 'NONE',  ( -210.0000000000000000, 12.00000000000001421, -126.4213562373080180 ) ) ;
#5355 = DIRECTION ( 'NONE',  ( -0.000000000000000000, -1.000000000000000000, -0.000000000000000000 ) ) ;
#5356 = CARTESIAN_POINT ( 'NONE',  ( -127.4999999999999716, -9.213203435596451385, -126.4213562373086575 ) ) ;
#5357 = CIRCLE ( 'NONE', #2604, 30.00000000000021316 ) ;
#5358 = CARTESIAN_POINT ( 'NONE',  ( 19.97493946039394430, 182.3862959170359659, -123.6698968802414953 ) ) ;
#5359 = VERTEX_POINT ( 'NONE', #10455 ) ;
#5360 = CARTESIAN_POINT ( 'NONE',  ( -19.95507986285562652, 178.2540685118973443, -123.3298867597350323 ) ) ;
#5361 = CARTESIAN_POINT ( 'NONE',  ( 0.000000000000000000, 24.00000000000001776, -159.6807709998038547 ) ) ;
#5362 = CARTESIAN_POINT ( 'NONE',  ( -1012.527716518106786, 86.38194213450564973, -154.8742214401233070 ) ) ;
#5363 = FACE_OUTER_BOUND ( 'NONE', #11938, .T. ) ;
#5364 = AXIS2_PLACEMENT_3D ( 'NONE', #9850, #10889, #8058 ) ;
#5365 = EDGE_CURVE ( 'NONE', #11420, #6480, #2024, .T. ) ;
#5366 = CARTESIAN_POINT ( 'NONE',  ( 1.387778780781445676E-14, 0.000000000000000000, 126.4213562373094959 ) ) ;
#5367 = DIRECTION ( 'NONE',  ( 0.000000000000000000, 0.000000000000000000, -1.000000000000000000 ) ) ;
#5368 = DIRECTION ( 'NONE',  ( -1.000000000000000000, 0.000000000000000000, 0.000000000000000000 ) ) ;
#5369 = ORIENTED_EDGE ( 'NONE', *, *, #1146, .F. ) ;
#5370 = CARTESIAN_POINT ( 'NONE',  ( 6.247927005943220505E-13, 152.0000000000000000, -66.42135623730948168 ) ) ;
#5371 = EDGE_CURVE ( 'NONE', #2194, #4285, #8780, .T. ) ;
#5372 = ORIENTED_EDGE ( 'NONE', *, *, #4260, .F. ) ;
#5373 = DIRECTION ( 'NONE',  ( 0.000000000000000000, 1.000000000000000000, 0.000000000000000000 ) ) ;
#5374 = CARTESIAN_POINT ( 'NONE',  ( -928.2641150402240555, 65.00826535581498433, -141.4553492942759476 ) ) ;
#5375 = CARTESIAN_POINT ( 'NONE',  ( 19.83195864043130641, 180.4357261996970010, -127.2679348835839335 ) ) ;
#5376 = ORIENTED_EDGE ( 'NONE', *, *, #10469, .F. ) ;
#5377 = CARTESIAN_POINT ( 'NONE',  ( -19.98227708713212181, 181.0992491550492787, -125.8737299293410530 ) ) ;
#5378 = CARTESIAN_POINT ( 'NONE',  ( 1.479627290717497352E-14, -58.00000000000000711, 118.9213562373094817 ) ) ;
#5379 = CIRCLE ( 'NONE', #249, 35.00000000000002842 ) ;
#5380 = EDGE_LOOP ( 'NONE', ( #3718, #7921 ) ) ;
#5381 = CARTESIAN_POINT ( 'NONE',  ( -370.9998549364893279, 58.67489986252060419, -138.4514685534600460 ) ) ;
#5382 = DIRECTION ( 'NONE',  ( 3.061276722312011504E-17, -1.000000000000000000, 0.000000000000000000 ) ) ;
#5383 = VERTEX_POINT ( 'NONE', #9707 ) ;
#5384 = ADVANCED_FACE ( 'NONE', ( #7550, #62, #10511, #4825, #4882, #9464, #1068, #1003, #11379, #3096, #8665, #8721, #8601, #2918, #123, #3898, #177, #3958, #10633, #7727, #11501, #6799, #2111, #5870, #1191, #4944 ), #7794, .F. ) ;
#5385 = EDGE_CURVE ( 'NONE', #8245, #7119, #2174, .T. ) ;
#5386 = ORIENTED_EDGE ( 'NONE', *, *, #3262, .T. ) ;
#5387 = CARTESIAN_POINT ( 'NONE',  ( -1017.158871447983074, 53.64146012065780411, -126.6442663926291061 ) ) ;
#5388 = ADVANCED_FACE ( 'NONE', ( #5297 ), #4272, .T. ) ;
#5389 = CYLINDRICAL_SURFACE ( 'NONE', #6026, 7.500000000000007105 ) ;
#5390 = AXIS2_PLACEMENT_3D ( 'NONE', #11279, #961, #4732 ) ;
#5391 = CARTESIAN_POINT ( 'NONE',  ( 35.00000000000000000, 12.00000000000002309, -159.6807709998040252 ) ) ;
#5392 = CARTESIAN_POINT ( 'NONE',  ( -818.8610518734294601, 79.33190776187021243, -154.5898210126322851 ) ) ;
#5393 = CARTESIAN_POINT ( 'NONE',  ( -795.0000000000080718, 82.00000000000049738, -94.48732055948593711 ) ) ;
#5394 = CARTESIAN_POINT ( 'NONE',  ( 4.285787411236815022E-15, 24.00000000000001776, -126.4213562373094959 ) ) ;
#5395 = ORIENTED_EDGE ( 'NONE', *, *, #6074, .F. ) ;
#5396 = CIRCLE ( 'NONE', #4042, 19.00000000000000000 ) ;
#5397 = CARTESIAN_POINT ( 'NONE',  ( 3.123963502971610252E-13, 164.0000000000000000, -88.92135623730946747 ) ) ;
#5398 =( NAMED_UNIT ( * ) PLANE_ANGLE_UNIT ( ) SI_UNIT ( $, .RADIAN. ) );
#5399 = EDGE_LOOP ( 'NONE', ( #7804, #4428 ) ) ;
#5400 = EDGE_CURVE ( 'NONE', #9244, #586, #7151, .T. ) ;
#5401 = DIRECTION ( 'NONE',  ( 0.000000000000000000, 0.000000000000000000, -1.000000000000000000 ) ) ;
#5402 = EDGE_CURVE ( 'NONE', #4019, #9416, #5168, .T. ) ;
#5403 = DIRECTION ( 'NONE',  ( 0.000000000000000000, -1.000000000000000000, -0.000000000000000000 ) ) ;
#5404 = CARTESIAN_POINT ( 'NONE',  ( 20.74227355824053021, 180.7311119294840580, -123.3990510803982943 ) ) ;
#5405 = EDGE_CURVE ( 'NONE', #1589, #7692, #1307, .T. ) ;
#5406 = AXIS2_PLACEMENT_3D ( 'NONE', #3463, #10445, #4874 ) ;
#5407 = AXIS2_PLACEMENT_3D ( 'NONE', #3981, #4736, #1024 ) ;
#5408 = DIRECTION ( 'NONE',  ( -0.000000000000000000, -1.000000000000000000, -0.000000000000000000 ) ) ;
#5409 = CARTESIAN_POINT ( 'NONE',  ( -19.92916319319399676, 178.5949286292980389, -122.9963005650378420 ) ) ;
#5410 = CARTESIAN_POINT ( 'NONE',  ( -828.6674387974358069, 77.37343372931279362, -144.1410586993679033 ) ) ;
#5411 = ORIENTED_EDGE ( 'NONE', *, *, #2933, .F. ) ;
#5412 = CARTESIAN_POINT ( 'NONE',  ( -370.0965291547436209, 56.26080251570542856, -130.6795707448060853 ) ) ;
#5413 = EDGE_LOOP ( 'NONE', ( #4039, #3106, #4883, #1124 ) ) ;
#5414 = CYLINDRICAL_SURFACE ( 'NONE', #11580, 5.000000000000115463 ) ;
#5415 = CARTESIAN_POINT ( 'NONE',  ( -1054.380968608932108, 114.0683136310379524, -122.7172756069792570 ) ) ;
#5416 = AXIS2_PLACEMENT_3D ( 'NONE', #4545, #12014, #7257 ) ;
#5417 = AXIS2_PLACEMENT_3D ( 'NONE', #2660, #9019, #11132 ) ;
#5418 = CARTESIAN_POINT ( 'NONE',  ( 6.899999999999999467, -10.39230484541326405, 0.000000000000000000 ) ) ;
#5419 = CARTESIAN_POINT ( 'NONE',  ( 3.123963502971610252E-13, -6.000000000000005329, -96.42135623730949590 ) ) ;
#5420 = CARTESIAN_POINT ( 'NONE',  ( -370.7822674372037000, 58.06085559963763387, -112.2852247942253712 ) ) ;
#5421 = CARTESIAN_POINT ( 'NONE',  ( 20.00026463111520414, 182.6897424871681324, -124.5631314607046818 ) ) ;
#5422 = EDGE_LOOP ( 'NONE', ( #4657, #11251, #1385, #4768 ) ) ;
#5423 = ORIENTED_EDGE ( 'NONE', *, *, #3078, .F. ) ;
#5424 = B_SPLINE_CURVE_WITH_KNOTS ( 'NONE', 3,
 ( #10800, #5047, #8827, #6109, #9877, #4134, #531, #4314, #7154, #5286, #6231, #9996, #1526, #290, #7466, #11974, #8341, #1649, #6535, #7216, #6342, #6286, #10181, #4436, #3690, #3549, #3614, #8411, #863, #1718, #7405, #2703, #7338, #5347, #11045, #9318, #5410, #597, #11909, #2571, #11179, #1783 ),
 .UNSPECIFIED., .F., .F.,
 ( 4, 2, 2, 2, 2, 2, 2, 2, 2, 2, 2, 2, 2, 2, 2, 2, 2, 2, 2, 2, 4 ),
 ( 0.000000000000000000, 0.0009975002171430115937, 0.001496250325714546230, 0.001995000434286080867, 0.002992500651429167054, 0.003990000868572252807, 0.004987501085715338560, 0.005486251194286759572, 0.005985001302858180584, 0.006982501520001022609, 0.007980001737143863766, 0.008478751845715450444, 0.008977501954287037123, 0.009975002171430533138, 0.01097250238857403262, 0.01197000260571752864, 0.01296750282286102465, 0.01396500304000452240, 0.01496250325714802015, 0.01546125336571982888, 0.01596000347429163760 ),
 .UNSPECIFIED. ) ;
#5425 = CIRCLE ( 'NONE', #914, 1.000000000000000888 ) ;
#5426 = FACE_BOUND ( 'NONE', #8123, .T. ) ;
#5427 = CARTESIAN_POINT ( 'NONE',  ( -819.8285638327245124, 78.67432280806536937, -159.6807709998044800 ) ) ;
#5428 = CARTESIAN_POINT ( 'NONE',  ( -1015.517346982278013, 86.95624952299075971, -154.8742214401231649 ) ) ;
#5429 = CARTESIAN_POINT ( 'NONE',  ( -826.0729559276804821, 74.19411019796237383, -143.0951037527842686 ) ) ;
#5430 = CARTESIAN_POINT ( 'NONE',  ( 0.8038475772933666441, 10.39230484541326938, -2.501782431774985704E-16 ) ) ;
#5431 = CARTESIAN_POINT ( 'NONE',  ( -2.775557561562891351E-14, 139.9999999999999716, -89.68077099980384048 ) ) ;
#5432 = FACE_OUTER_BOUND ( 'NONE', #10129, .T. ) ;
#5433 = ORIENTED_EDGE ( 'NONE', *, *, #7212, .T. ) ;
#5434 = DIRECTION ( 'NONE',  ( 0.000000000000000000, 1.000000000000000000, 0.000000000000000000 ) ) ;
#5435 = ORIENTED_EDGE ( 'NONE', *, *, #10382, .T. ) ;
#5436 = DIRECTION ( 'NONE',  ( 1.000000000000000000, 0.000000000000000000, 0.000000000000000000 ) ) ;
#5437 = CARTESIAN_POINT ( 'NONE',  ( -1056.743458481019616, 64.45745743522664384, -152.5758913445293956 ) ) ;
#5438 = AXIS2_PLACEMENT_3D ( 'NONE', #6932, #5066, #246 ) ;
#5439 = CARTESIAN_POINT ( 'NONE',  ( 19.93046079246938618, 182.1848923560334015, -126.3549534181600791 ) ) ;
#5440 = VERTEX_POINT ( 'NONE', #11750 ) ;
#5441 = EDGE_CURVE ( 'NONE', #11262, #9215, #5059, .T. ) ;
#5442 = ORIENTED_EDGE ( 'NONE', *, *, #1619, .F. ) ;
#5443 = CARTESIAN_POINT ( 'NONE',  ( -19.83578844811568587, 180.6327930221633835, -127.2386752689097023 ) ) ;
#5444 = ORIENTED_EDGE ( 'NONE', *, *, #3077, .T. ) ;
#5445 = CARTESIAN_POINT ( 'NONE',  ( -381.0219023890770131, 65.38716504393917717, -135.8359694540845055 ) ) ;
#5446 = PRODUCT_DEFINITION_FORMATION_WITH_SPECIFIED_SOURCE ( 'ANY', '', #7932, .NOT_KNOWN. ) ;
#5447 = DIRECTION ( 'NONE',  ( -1.000000000000000000, 0.000000000000000000, 0.000000000000000000 ) ) ;
#5448 = ORIENTED_EDGE ( 'NONE', *, *, #1794, .T. ) ;
#5449 = AXIS2_PLACEMENT_3D ( 'NONE', #3281, #7057, #9901 ) ;
#5450 = FACE_OUTER_BOUND ( 'NONE', #1208, .T. ) ;
#5451 = LINE ( 'NONE', #8321, #2088 ) ;
#5452 = ADVANCED_FACE ( 'NONE', ( #3263 ), #2352, .F. ) ;
#5453 = CARTESIAN_POINT ( 'NONE',  ( -19.00000000000000000, 197.0000000000000000, -124.6807709998038405 ) ) ;
#5454 = DIRECTION ( 'NONE',  ( -1.000000000000000000, 0.000000000000000000, 0.000000000000000000 ) ) ;
#5455 = DIRECTION ( 'NONE',  ( 0.000000000000000000, 1.000000000000000000, 0.000000000000000000 ) ) ;
#5456 = ADVANCED_FACE ( 'NONE', ( #5994 ), #1539, .F. ) ;
#5457 = AXIS2_PLACEMENT_3D ( 'NONE', #9299, #772, #6579 ) ;
#5458 = CARTESIAN_POINT ( 'NONE',  ( -994.1998135634719347, 88.30642396300639518, -95.06748246948001224 ) ) ;
#5459 = FACE_OUTER_BOUND ( 'NONE', #434, .T. ) ;
#5460 = CARTESIAN_POINT ( 'NONE',  ( -21.06729583384051097, 179.4139655881280078, -126.1965993184190040 ) ) ;
#5461 = CARTESIAN_POINT ( 'NONE',  ( -1048.438004920982848, 39.66697241395321782, -126.6442663926296603 ) ) ;
#5462 = CARTESIAN_POINT ( 'NONE',  ( -824.1603064692830003, 83.67418067986891117, -144.6105757924098327 ) ) ;
#5463 = VERTEX_POINT ( 'NONE', #8040 ) ;
#5464 = FACE_OUTER_BOUND ( 'NONE', #9779, .T. ) ;
#5465 = EDGE_CURVE ( 'NONE', #3503, #1233, #2227, .T. ) ;
#5466 = CARTESIAN_POINT ( 'NONE',  ( 213.8374762401696785, 8.587870355341205825E-13, 18.10678370264077230 ) ) ;
#5467 = ORIENTED_EDGE ( 'NONE', *, *, #4258, .T. ) ;
#5468 = FACE_OUTER_BOUND ( 'NONE', #4286, .T. ) ;
#5469 = CARTESIAN_POINT ( 'NONE',  ( -1047.151245865161172, 77.61790247226321071, -94.48732055948626396 ) ) ;
#5470 = AXIS2_PLACEMENT_3D ( 'NONE', #6156, #2441, #5401 ) ;
#5471 = LINE ( 'NONE', #5539, #11626 ) ;
#5472 = CARTESIAN_POINT ( 'NONE',  ( 0.8038475772933614261, 5.196152422706624030, -9.000000000000000000 ) ) ;
#5473 = CARTESIAN_POINT ( 'NONE',  ( 21.06714545844871722, 179.4370239411119030, -126.2109676220344596 ) ) ;
#5474 = AXIS2_PLACEMENT_3D ( 'NONE', #2247, #11990, #9782 ) ;
#5475 = LINE ( 'NONE', #2629, #7131 ) ;
#5476 = CARTESIAN_POINT ( 'NONE',  ( -821.2975544693601933, 74.34970510072395200, -106.2007125858225720 ) ) ;
#5477 = DIRECTION ( 'NONE',  ( 2.040851148208007875E-17, -1.000000000000000000, -0.000000000000000000 ) ) ;
#5478 = VECTOR ( 'NONE', #4462, 1000.000000000000000 ) ;
#5479 = EDGE_CURVE ( 'NONE', #6719, #11656, #8729, .T. ) ;
#5480 = EDGE_LOOP ( 'NONE', ( #6150, #675 ) ) ;
#5481 = ORIENTED_EDGE ( 'NONE', *, *, #3348, .F. ) ;
#5482 = CARTESIAN_POINT ( 'NONE',  ( 0.000000000000000000, 152.0000000000000284, -126.4213562373094959 ) ) ;
#5483 = CARTESIAN_POINT ( 'NONE',  ( -373.1519908486758368, 97.99425499239711712, -100.8725093751089332 ) ) ;
#5484 = CARTESIAN_POINT ( 'NONE',  ( -818.8609295919769693, 78.01955378747423708, -154.6506939777316632 ) ) ;
#5485 = ORIENTED_EDGE ( 'NONE', *, *, #6929, .F. ) ;
#5486 = PLANE ( 'NONE',  #2899 ) ;
#5487 = CARTESIAN_POINT ( 'NONE',  ( -954.0441199534441239, 124.9954171138387977, -122.7172756069788875 ) ) ;
#5488 = ADVANCED_FACE ( 'NONE', ( #7041 ), #8889, .F. ) ;
#5489 = DIRECTION ( 'NONE',  ( 1.000000000000000000, 0.000000000000000000, 0.000000000000000000 ) ) ;
#5490 = DIRECTION ( 'NONE',  ( -1.000000000000000000, 0.000000000000000000, 0.000000000000000000 ) ) ;
#5491 = DIRECTION ( 'NONE',  ( -8.163404592832031500E-17, 1.000000000000000000, 0.000000000000000000 ) ) ;
#5492 = CIRCLE ( 'NONE', #9642, 7.500000000000007105 ) ;
#5493 = CARTESIAN_POINT ( 'NONE',  ( 21.05011458093100529, 181.5921831639467996, -125.4765988369088916 ) ) ;
#5494 = EDGE_LOOP ( 'NONE', ( #11595, #3960, #4951, #2328 ) ) ;
#5495 = ORIENTED_EDGE ( 'NONE', *, *, #11065, .T. ) ;
#5496 = APPLICATION_CONTEXT ( 'automotive_design' ) ;
#5497 = EDGE_CURVE ( 'NONE', #4307, #1330, #11862, .T. ) ;
#5498 = AXIS2_PLACEMENT_3D ( 'NONE', #3102, #1490, #9954 ) ;
#5499 = CARTESIAN_POINT ( 'NONE',  ( 7.500000000000000000, 5.196152422706624918, 8.999999999999998224 ) ) ;
#5500 = LINE ( 'NONE', #2651, #8184 ) ;
#5501 = CARTESIAN_POINT ( 'NONE',  ( -1037.656130532295037, 99.96792753513321372, -149.7857175106633747 ) ) ;
#5502 = CARTESIAN_POINT ( 'NONE',  ( -379.1553463010024529, 102.0109503771648605, -124.6625911296856088 ) ) ;
#5503 = CARTESIAN_POINT ( 'NONE',  ( 87.04832655144112152, 12.00000000000000000, -217.9289243767383368 ) ) ;
#5504 = CYLINDRICAL_SURFACE ( 'NONE', #7607, 7.500000000000007105 ) ;
#5505 = ORIENTED_EDGE ( 'NONE', *, *, #7613, .F. ) ;
#5506 = CARTESIAN_POINT ( 'NONE',  ( -818.9900958282657939, 77.37130366011599847, -94.69300966023514832 ) ) ;
#5507 = AXIS2_PLACEMENT_3D ( 'NONE', #11623, #353, #4014 ) ;
#5508 = CARTESIAN_POINT ( 'NONE',  ( -374.1876840878753683, 94.02523439044611564, -140.7929094221022979 ) ) ;
#5509 = ORIENTED_EDGE ( 'NONE', *, *, #8908, .F. ) ;
#5510 = CARTESIAN_POINT ( 'NONE',  ( -995.4135022096103285, 71.70161378084171133, -154.2940595301282656 ) ) ;
#5511 = CIRCLE ( 'NONE', #12235, 7.500000000000007105 ) ;
#5512 = EDGE_LOOP ( 'NONE', ( #9203, #5699, #4179, #10085 ) ) ;
#5513 = ORIENTED_EDGE ( 'NONE', *, *, #2447, .F. ) ;
#5514 = DIRECTION ( 'NONE',  ( 1.000000000000000000, 0.000000000000000000, -0.000000000000000000 ) ) ;
#5515 = AXIS2_PLACEMENT_3D ( 'NONE', #48, #5678, #7600 ) ;
#5516 = ORIENTED_EDGE ( 'NONE', *, *, #10153, .T. ) ;
#5517 = CARTESIAN_POINT ( 'NONE',  ( -379.1358231506008565, 61.95672027140099658, -124.6842552236176687 ) ) ;
#5518 = COLOUR_RGB ( '', 0.40784314, 0.44705882, 0.49803922) ;
#5519 = DIRECTION ( 'NONE',  ( 1.000000000000000000, 0.000000000000000000, -0.000000000000000000 ) ) ;
#5520 = CIRCLE ( 'NONE', #2766, 7.500000000000007105 ) ;
#5521 = DIRECTION ( 'NONE',  ( -0.7071067811865477948, 0.000000000000000000, -0.7071067811865473507 ) ) ;
#5522 = ORIENTED_EDGE ( 'NONE', *, *, #1344, .T. ) ;
#5523 = CARTESIAN_POINT ( 'NONE',  ( -19.91081574664456610, 181.5182364730087272, -122.7941294590837913 ) ) ;
#5524 = FACE_OUTER_BOUND ( 'NONE', #4421, .T. ) ;
#5525 = CARTESIAN_POINT ( 'NONE',  ( -30.00000000000000000, -492.9999999999998863, -30.00000000000000000 ) ) ;
#5526 = CARTESIAN_POINT ( 'NONE',  ( -1026.651933061283898, 84.71212313386838844, -94.48732055948616448 ) ) ;
#5527 = LINE ( 'NONE', #6272, #12071 ) ;
#5528 = CARTESIAN_POINT ( 'NONE',  ( -1065.000000000000682, 52.38665522077219805, -130.5712005305403238 ) ) ;
#5529 = CARTESIAN_POINT ( 'NONE',  ( -820.0597211274506435, 81.97619047958284000, -144.6820902952100596 ) ) ;
#5530 = ORIENTED_EDGE ( 'NONE', *, *, #403, .F. ) ;
#5531 = CARTESIAN_POINT ( 'NONE',  ( -827.1410867119011527, 82.43389265416584522, -144.6774099844741670 ) ) ;
#5532 = EDGE_CURVE ( 'NONE', #11915, #10880, #2212, .T. ) ;
#5533 = DIRECTION ( 'NONE',  ( 1.000000000000000000, 0.000000000000000000, 0.000000000000000000 ) ) ;
#5534 = CARTESIAN_POINT ( 'NONE',  ( -370.2891325637493196, 107.2458676303090925, -116.4427368508418823 ) ) ;
#5535 = ORIENTED_EDGE ( 'NONE', *, *, #5296, .T. ) ;
#5536 = LINE ( 'NONE', #11237, #11392 ) ;
#5538 = ADVANCED_FACE ( 'NONE', ( #4089 ), #6164, .T. ) ;
#5537 = CARTESIAN_POINT ( 'NONE',  ( -1016.652307257391612, 63.31440937415304404, -103.3307627799640045 ) ) ;
#5539 = CARTESIAN_POINT ( 'NONE',  ( 9.371890508914830252E-13, -6.000000000000006217, -28.92135623730948524 ) ) ;
#5540 = DIRECTION ( 'NONE',  ( -0.7071067811865472397, 0.000000000000000000, 0.7071067811865479058 ) ) ;
#5541 = CARTESIAN_POINT ( 'NONE',  ( 19.87268743161337170, 178.9255784920988503, -126.9338343023757290 ) ) ;
#5542 = DIRECTION ( 'NONE',  ( 0.000000000000000000, 0.000000000000000000, 1.000000000000000000 ) ) ;
#5543 = EDGE_CURVE ( 'NONE', #6424, #1735, #4785, .T. ) ;
#5544 = DIRECTION ( 'NONE',  ( -0.000000000000000000, 1.000000000000000000, 7.930164461608263644E-17 ) ) ;
#5545 = CARTESIAN_POINT ( 'NONE',  ( -20.00054430879287892, 177.7104753434648785, -124.6347125233424009 ) ) ;
#5546 = DIRECTION ( 'NONE',  ( -0.04986130261928722884, -0.8527687809245380057, 0.5199031224964757447 ) ) ;
#5547 = ORIENTED_EDGE ( 'NONE', *, *, #11535, .T. ) ;
#5548 = CARTESIAN_POINT ( 'NONE',  ( -372.2568423259174892, 62.53082544746772697, -144.9467117470782114 ) ) ;
#5549 = ITEM_DEFINED_TRANSFORMATION ( 'NONE', 'NONE', #4855,  #11957 ) ;
#5550 = CARTESIAN_POINT ( 'NONE',  ( -383.4981472370314464, 92.28971772028073417, -107.5277044879749155 ) ) ;
#5551 = EDGE_LOOP ( 'NONE', ( #11276, #10366, #9344, #2663 ) ) ;
#5552 = CARTESIAN_POINT ( 'NONE',  ( -1045.967528061859412, 112.8272211019270230, -113.1262384684098663 ) ) ;
#5553 = CIRCLE ( 'NONE', #7127, 45.00000000000000711 ) ;
#5554 = DIRECTION ( 'NONE',  ( 0.000000000000000000, 0.000000000000000000, 1.000000000000000000 ) ) ;
#5555 = EDGE_CURVE ( 'NONE', #5299, #7650, #1231, .T. ) ;
#5556 = CARTESIAN_POINT ( 'NONE',  ( 19.85181743999062576, 181.1549164222419961, -127.1121716299344087 ) ) ;
#5557 = VERTEX_POINT ( 'NONE', #543 ) ;
#5558 = ORIENTED_EDGE ( 'NONE', *, *, #8202, .T. ) ;
#5559 = CARTESIAN_POINT ( 'NONE',  ( -52.49999999999997868, 24.00000000000001421, -126.4213562373090696 ) ) ;
#5560 = CARTESIAN_POINT ( 'NONE',  ( 1.387778780781445676E-14, -492.9999999999998863, 133.9213562373095101 ) ) ;
#5561 = CARTESIAN_POINT ( 'NONE',  ( -974.7984820115178763, 96.63273410478066694, -152.5758913445288272 ) ) ;
#5562 = SURFACE_STYLE_USAGE ( .BOTH. , #1800 ) ;
#5563 = CARTESIAN_POINT ( 'NONE',  ( 0.8038475772933614261, 5.196152422706624030, -9.000000000000000000 ) ) ;
#5564 = CARTESIAN_POINT ( 'NONE',  ( -1055.469533842436022, 91.91071092603651493, -152.5758913445291398 ) ) ;
#5565 = ORIENTED_EDGE ( 'NONE', *, *, #11914, .T. ) ;
#5566 = DIRECTION ( 'NONE',  ( 0.000000000000000000, 1.000000000000000000, 0.000000000000000000 ) ) ;
#5567 = CIRCLE ( 'NONE', #3004, 7.500000000000007105 ) ;
#5568 = CARTESIAN_POINT ( 'NONE',  ( -374.4727959898146423, 91.87416495705461728, -142.1456732492470394 ) ) ;
#5569 = VERTEX_POINT ( 'NONE', #4326 ) ;
#5570 = CARTESIAN_POINT ( 'NONE',  ( -953.5758047008371250, 72.53746257253824581, -152.5758913445294525 ) ) ;
#5571 = EDGE_CURVE ( 'NONE', #5951, #3434, #8098, .T. ) ;
#5572 = ORIENTED_EDGE ( 'NONE', *, *, #9507, .F. ) ;
#5573 = AXIS2_PLACEMENT_3D ( 'NONE', #6642, #9484, #4677 ) ;
#5574 = EDGE_LOOP ( 'NONE', ( #9149, #3446, #8240, #3269 ) ) ;
#5575 = AXIS2_PLACEMENT_3D ( 'NONE', #10572, #11441, #9523 ) ;
#5576 = ADVANCED_FACE ( 'NONE', ( #10007 ), #7886, .F. ) ;
#5577 = CARTESIAN_POINT ( 'NONE',  ( -828.8285638327246261, 78.99577924834096621, -144.4565372401591219 ) ) ;
#5578 = CARTESIAN_POINT ( 'NONE',  ( -20.93827155636993353, 181.6390200720728387, -124.4080817122161307 ) ) ;
#5579 = CARTESIAN_POINT ( 'NONE',  ( -828.7963533401381255, 78.01901522663844446, -105.0781937692942734 ) ) ;
#5580 = EDGE_LOOP ( 'NONE', ( #7078, #3513 ) ) ;
#5581 = CARTESIAN_POINT ( 'NONE',  ( -370.4278987528730909, 57.11177549475814175, -134.4195693297641014 ) ) ;
#5582 = DIRECTION ( 'NONE',  ( -0.000000000000000000, -1.000000000000000000, -0.000000000000000000 ) ) ;
#5583 = CARTESIAN_POINT ( 'NONE',  ( -818.8285638327242850, 78.67432280806536937, -90.68077099980378364 ) ) ;
#5584 = AXIS2_PLACEMENT_3D ( 'NONE', #2941, #10411, #7818 ) ;
#5585 = CARTESIAN_POINT ( 'NONE',  ( 2.186774452080127126E-12, 152.0000000000000000, 83.57864376269051832 ) ) ;
#5586 = DIRECTION ( 'NONE',  ( -0.000000000000000000, 1.000000000000000000, 0.000000000000000000 ) ) ;
#5587 = CARTESIAN_POINT ( 'NONE',  ( 21.05815107556387389, 178.8909823731209485, -125.6365553545643081 ) ) ;
#5588 = VECTOR ( 'NONE', #7185, 1000.000000000000000 ) ;
#5589 = CARTESIAN_POINT ( 'NONE',  ( -997.0443963278638648, 49.75991663364290929, -103.3307627799637487 ) ) ;
#5590 = DIRECTION ( 'NONE',  ( 2.081668171172161734E-17, 4.930380657631307143E-31, -1.000000000000000000 ) ) ;
#5591 = DIRECTION ( 'NONE',  ( -1.000000000000000000, -8.163404592832031500E-17, 0.000000000000000000 ) ) ;
#5592 = CARTESIAN_POINT ( 'NONE',  ( -957.2086549536780922, 47.65337959301152893, -122.7172756069790012 ) ) ;
#5593 = CARTESIAN_POINT ( 'NONE',  ( -824.4888212380200230, 83.64126188030940057, -144.6134169528915265 ) ) ;
#5594 = ORIENTED_EDGE ( 'NONE', *, *, #5948, .F. ) ;
#5595 = CARTESIAN_POINT ( 'NONE',  ( -818.8602280653254866, 79.32430977885819345, -144.5036099591915502 ) ) ;
#5596 = DIRECTION ( 'NONE',  ( -0.02173091171106836944, -1.212631691043329670E-16, -0.9997638558560747457 ) ) ;
#5597 = CARTESIAN_POINT ( 'NONE',  ( -370.0989827543548927, 107.7329936528643657, -118.6480030875499097 ) ) ;
#5598 = ORIENTED_EDGE ( 'NONE', *, *, #10176, .T. ) ;
#5599 = CARTESIAN_POINT ( 'NONE',  ( -1057.521967982379238, 48.25222617154000204, -107.9061927053324723 ) ) ;
#5600 = AXIS2_PLACEMENT_3D ( 'NONE', #2204, #9801, #5211 ) ;
#5601 = CARTESIAN_POINT ( 'NONE',  ( 19.90865200055593220, 181.4799304009739558, -122.7714319726113104 ) ) ;
#5602 = CARTESIAN_POINT ( 'NONE',  ( 35.00000000000000000, 163.9999999999999716, 190.3192290001959748 ) ) ;
#5603 = EDGE_CURVE ( 'NONE', #867, #1589, #11696, .T. ) ;
#5604 = CARTESIAN_POINT ( 'NONE',  ( -1025.044148074454370, 113.2108726315405960, -107.9061927053325007 ) ) ;
#5605 = LINE ( 'NONE', #7403, #6512 ) ;
#5606 = CARTESIAN_POINT ( 'NONE',  ( -20.00030393798869355, 177.7000510669864184, -124.7934183480526968 ) ) ;
#5607 = AXIS2_PLACEMENT_3D ( 'NONE', #11543, #10490, #9560 ) ;
#5608 = EDGE_LOOP ( 'NONE', ( #103, #11015, #1070, #9434 ) ) ;
#5609 = DIRECTION ( 'NONE',  ( 0.7071067811865477948, -0.000000000000000000, 0.7071067811865473507 ) ) ;
#5610 = CARTESIAN_POINT ( 'NONE',  ( -373.8485616844952801, 96.00934940626343916, -110.2553559621317589 ) ) ;
#5611 = ORIENTED_EDGE ( 'NONE', *, *, #4362, .T. ) ;
#5612 = DIRECTION ( 'NONE',  ( 0.000000000000000000, -1.156482317317870246E-16, 1.000000000000000000 ) ) ;
#5613 = AXIS2_PLACEMENT_3D ( 'NONE', #10984, #10117, #1585 ) ;
#5614 = CIRCLE ( 'NONE', #7596, 7.500000000000013323 ) ;
#5615 = VECTOR ( 'NONE', #1216, 1000.000000000000000 ) ;
#5616 = ORIENTED_EDGE ( 'NONE', *, *, #2750, .F. ) ;
#5617 = VERTEX_POINT ( 'NONE', #12101 ) ;
#5618 = EDGE_CURVE ( 'NONE', #1440, #5971, #9714, .T. ) ;
#5619 = DIRECTION ( 'NONE',  ( -0.000000000000000000, 1.000000000000000000, -0.000000000000000000 ) ) ;
#5620 = DIRECTION ( 'NONE',  ( -1.000000000000000000, -0.000000000000000000, -0.000000000000000000 ) ) ;
#5621 = CARTESIAN_POINT ( 'NONE',  ( -853.2189900670995257, 91.12674563889149226, -152.5758913445289693 ) ) ;
#5622 = CARTESIAN_POINT ( 'NONE',  ( -370.4476841044511275, 106.8318587325821341, -114.9410180965496977 ) ) ;
#5623 = CIRCLE ( 'NONE', #9175, 8.500000000000007105 ) ;
#5624 = CARTESIAN_POINT ( 'NONE',  ( -262.5000000000000000, -9.213203435596478030, -126.4213562373076059 ) ) ;
#5625 = AXIS2_PLACEMENT_3D ( 'NONE', #11775, #11718, #390 ) ;
#5626 = CARTESIAN_POINT ( 'NONE',  ( -1061.468168685229102, 92.73456844357778550, -152.5758913445291398 ) ) ;
#5627 = DIRECTION ( 'NONE',  ( 0.000000000000000000, 0.000000000000000000, 1.000000000000000000 ) ) ;
#5628 = ORIENTED_EDGE ( 'NONE', *, *, #2231, .T. ) ;
#5629 = CARTESIAN_POINT ( 'NONE',  ( -6.106226635438360972E-13, 12.00000000000000000, -244.6807709998039400 ) ) ;
#5630 = CARTESIAN_POINT ( 'NONE',  ( -45.53315400109751465, 12.00000000000000000, -237.8419396193594650 ) ) ;
#5631 = CARTESIAN_POINT ( 'NONE',  ( -374.0189381182528905, 95.05895014862441883, -139.9740603887058228 ) ) ;
#5632 = VERTEX_POINT ( 'NONE', #7522 ) ;
#5633 = CARTESIAN_POINT ( 'NONE',  ( -1047.151245865163673, 77.61790247226322492, -154.8742214401233070 ) ) ;
#5634 = CARTESIAN_POINT ( 'NONE',  ( -1054.380968608929606, 114.0683136310380803, -126.6442663926291345 ) ) ;
#5635 = DIRECTION ( 'NONE',  ( -1.000000000000000000, -3.061276722312011504E-17, 0.000000000000000000 ) ) ;
#5636 = ORIENTED_EDGE ( 'NONE', *, *, #8356, .F. ) ;
#5637 = VECTOR ( 'NONE', #8513, 1000.000000000000000 ) ;
#5638 = ORIENTED_EDGE ( 'NONE', *, *, #8556, .T. ) ;
#5639 = CARTESIAN_POINT ( 'NONE',  ( -826.9035580924005444, 74.71835857218601973, -106.0523996049648474 ) ) ;
#5640 = PLANE ( 'NONE',  #2130 ) ;
#5641 = CARTESIAN_POINT ( 'NONE',  ( -1021.293373424891683, 59.24127555818969171, -141.4553492942756918 ) ) ;
#5642 = ORIENTED_EDGE ( 'NONE', *, *, #5852, .T. ) ;
#5643 = EDGE_CURVE ( 'NONE', #7353, #2620, #4198, .T. ) ;
#5644 = CARTESIAN_POINT ( 'NONE',  ( -374.2711669801677772, 71.91685023077710071, -152.3836689249183678 ) ) ;
#5645 = CARTESIAN_POINT ( 'NONE',  ( -240.0000000000000000, -9.213203435596478030, -126.4213562373078190 ) ) ;
#5646 = CARTESIAN_POINT ( 'NONE',  ( -384.0215091375642373, 73.67838221987805980, -106.4912323260315787 ) ) ;
#5647 = CARTESIAN_POINT ( 'NONE',  ( 20.00000000000000355, 168.0000000000000000, -124.6807709998038405 ) ) ;
#5648 =( GEOMETRIC_REPRESENTATION_CONTEXT ( 3 ) GLOBAL_UNCERTAINTY_ASSIGNED_CONTEXT ( ( #12226 ) ) GLOBAL_UNIT_ASSIGNED_CONTEXT ( ( #8398, #5398, #2689 ) ) REPRESENTATION_CONTEXT ( 'NONE', 'WORKASPACE' ) );
#5649 = EDGE_CURVE ( 'NONE', #1185, #915, #10707, .T. ) ;
#5650 = CARTESIAN_POINT ( 'NONE',  ( 45.53315400109643463, 0.000000000000000000, -237.8419396193597208 ) ) ;
#5651 = DIRECTION ( 'NONE',  ( -0.3117078928809505767, -5.319854888938801199E-14, 0.9501779778103246477 ) ) ;
#5652 = CARTESIAN_POINT ( 'NONE',  ( -853.6888141844383426, 53.84495383942796565, -96.78565065507952170 ) ) ;
#5653 = CARTESIAN_POINT ( 'NONE',  ( -821.3208927675284485, 83.01261617298027318, -104.7055743826754224 ) ) ;
#5654 = CARTESIAN_POINT ( 'NONE',  ( -817.1493800258448346, 27.50875274330015685, -122.7172756069792001 ) ) ;
#5655 = CIRCLE ( 'NONE', #5449, 7.500000000000020428 ) ;
#5656 = EDGE_CURVE ( 'NONE', #11947, #10902, #242, .T. ) ;
#5657 = ORIENTED_EDGE ( 'NONE', *, *, #4058, .T. ) ;
#5658 = CARTESIAN_POINT ( 'NONE',  ( -828.3216978517729103, 80.87401637003858923, -144.6495766896180442 ) ) ;
#5659 = DIRECTION ( 'NONE',  ( 0.9994711065474020106, -8.783834896913952960E-16, -0.03251933543158296025 ) ) ;
#5660 = CARTESIAN_POINT ( 'NONE',  ( -373.7386929379060234, 95.23712357076890100, -98.76709413358776146 ) ) ;
#5661 = ORIENTED_EDGE ( 'NONE', *, *, #11144, .F. ) ;
#5662 = CARTESIAN_POINT ( 'NONE',  ( -997.4616017999825317, 44.34671234275855767, -107.9061927053325007 ) ) ;
#5663 = CYLINDRICAL_SURFACE ( 'NONE', #11422, 5.000000000000115463 ) ;
#5664 = CARTESIAN_POINT ( 'NONE',  ( 19.97926089986212261, 179.5776042405117323, -126.0284158974866813 ) ) ;
#5665 = CIRCLE ( 'NONE', #7244, 11.50000000000003730 ) ;
#5666 =( REPRESENTATION_RELATIONSHIP ('NONE','NONE', #12149, #690 ) REPRESENTATION_RELATIONSHIP_WITH_TRANSFORMATION ( #1653 )SHAPE_REPRESENTATION_RELATIONSHIP( ) );
#5667 = CARTESIAN_POINT ( 'NONE',  ( 2.186774452080127126E-12, 163.9999999999999716, 83.57864376269051832 ) ) ;
#5668 = VERTEX_POINT ( 'NONE', #9616 ) ;
#5669 = FACE_OUTER_BOUND ( 'NONE', #3111, .T. ) ;
#5670 = CARTESIAN_POINT ( 'NONE',  ( -374.5417925368921601, 91.27339439224303419, -106.8924592036498638 ) ) ;
#5671 = TOROIDAL_SURFACE ( 'NONE', #332, 10.00000000000003730, 1.499999999999998002 ) ;
#5672 = ORIENTED_EDGE ( 'NONE', *, *, #11302, .T. ) ;
#5673 = CARTESIAN_POINT ( 'NONE',  ( -1031.086615573502741, 111.8776252365149730, -107.9061927053324723 ) ) ;
#5674 = DIRECTION ( 'NONE',  ( 0.000000000000000000, 0.000000000000000000, 1.000000000000000000 ) ) ;
#5675 = AXIS2_PLACEMENT_3D ( 'NONE', #7255, #1820, #7685 ) ;
#5676 = CARTESIAN_POINT ( 'NONE',  ( -19.91081574664475795, 181.5182364730088125, -122.7941294590836492 ) ) ;
#5677 = EDGE_LOOP ( 'NONE', ( #1028, #5535, #9840, #10251, #7438 ) ) ;
#5678 = DIRECTION ( 'NONE',  ( 0.000000000000000000, 1.000000000000000000, -0.000000000000000000 ) ) ;
#5679 = CARTESIAN_POINT ( 'NONE',  ( 28.53314250459842327, 180.2041921146317236, -137.7978499286132319 ) ) ;
#5680 = CARTESIAN_POINT ( 'NONE',  ( -1054.913455627173789, 103.6024512377076974, -146.0307792196445291 ) ) ;
#5681 = CARTESIAN_POINT ( 'NONE',  ( -144.0488662551579182, 12.00000000000000000, -139.4077238332691877 ) ) ;
#5682 = ORIENTED_EDGE ( 'NONE', *, *, #639, .T. ) ;
#5683 = DIRECTION ( 'NONE',  ( 0.000000000000000000, 5.522905491341382306E-16, 1.000000000000000000 ) ) ;
#5684 = EDGE_CURVE ( 'NONE', #495, #9395, #3391, .T. ) ;
#5685 = CARTESIAN_POINT ( 'NONE',  ( -383.5692087195515683, 92.05770259072330930, -141.9802856064553396 ) ) ;
#5686 = ORIENTED_EDGE ( 'NONE', *, *, #651, .T. ) ;
#5687 = CARTESIAN_POINT ( 'NONE',  ( -975.5821371384174654, 62.83201726680850641, -152.5758913445291682 ) ) ;
#5688 = EDGE_CURVE ( 'NONE', #7974, #6035, #6954, .T. ) ;
#5689 = DIRECTION ( 'NONE',  ( 0.000000000000000000, 1.000000000000000000, -0.000000000000000000 ) ) ;
#5690 = VECTOR ( 'NONE', #2085, 1000.000000000000000 ) ;
#5691 = CARTESIAN_POINT ( 'NONE',  ( 14.74749198504303571, 180.2041921146325762, -184.6327933705058228 ) ) ;
#5692 = EDGE_LOOP ( 'NONE', ( #6705, #3014 ) ) ;
#5693 = CARTESIAN_POINT ( 'NONE',  ( 19.94029851291840316, 178.4426130827685029, -123.1320176715209840 ) ) ;
#5694 = VECTOR ( 'NONE', #472, 1000.000000000000000 ) ;
#5695 = ADVANCED_FACE ( 'NONE', ( #3065, #6768, #9678, #10542, #4914 ), #4854, .T. ) ;
#5696 = CARTESIAN_POINT ( 'NONE',  ( -827.6030183929074155, 81.96987526947719971, -144.6820941065185195 ) ) ;
#5697 = CARTESIAN_POINT ( 'NONE',  ( -19.99104260667089861, 181.5188412912357308, -125.4148505090950749 ) ) ;
#5698 = CARTESIAN_POINT ( 'NONE',  ( -854.0393178910245524, 26.93106345811121827, -136.2353035311989515 ) ) ;
#5699 = ORIENTED_EDGE ( 'NONE', *, *, #3479, .T. ) ;
#5700 = CARTESIAN_POINT ( 'NONE',  ( -374.6542199234099826, 73.81176977798163819, -142.9951582143055475 ) ) ;
#5701 = CARTESIAN_POINT ( 'NONE',  ( 13.32222501832753991, 180.2041921146325762, -184.1652315311844177 ) ) ;
#5702 = CARTESIAN_POINT ( 'NONE',  ( -373.4583060517632020, 67.32383868152314221, -99.73118028973054550 ) ) ;
#5703 = DIRECTION ( 'NONE',  ( -8.163404592832030268E-17, 1.000000000000000000, -0.000000000000000000 ) ) ;
#5704 = CIRCLE ( 'NONE', #8858, 8.999999999999998224 ) ;
#5705 = ADVANCED_FACE ( 'NONE', ( #11539 ), #4060, .F. ) ;
#5706 = DIRECTION ( 'NONE',  ( 0.000000000000000000, 0.000000000000000000, 1.000000000000000000 ) ) ;
#5707 = AXIS2_PLACEMENT_3D ( 'NONE', #3025, #1985, #9636 ) ;
#5708 = CARTESIAN_POINT ( 'NONE',  ( -902.4158961391592584, 71.79205886009090420, -99.57582448894511629 ) ) ;
#5709 = CIRCLE ( 'NONE', #1373, 7.500000000000007105 ) ;
#5710 = CARTESIAN_POINT ( 'NONE',  ( 0.5584673446548709119, -5.621163452808895400, -8.263859302085698744 ) ) ;
#5711 = DIRECTION ( 'NONE',  ( 2.040851148208007875E-17, -1.000000000000000000, -0.000000000000000000 ) ) ;
#5712 = ORIENTED_EDGE ( 'NONE', *, *, #5603, .F. ) ;
#5713 = CARTESIAN_POINT ( 'NONE',  ( -384.9053341376281310, 79.33775245455765912, -104.8495957246331898 ) ) ;
#5714 = EDGE_LOOP ( 'NONE', ( #8458, #4071, #9918, #3495 ) ) ;
#5715 = CARTESIAN_POINT ( 'NONE',  ( -828.5766943389837706, 80.27470094935036116, -144.6085013259155687 ) ) ;
#5716 = APPLICATION_PROTOCOL_DEFINITION ( 'draft international standard', 'automotive_design', 1998, #5496 ) ;
#5717 = DIRECTION ( 'NONE',  ( 0.000000000000000000, 1.000000000000000000, -0.000000000000000000 ) ) ;
#5718 = DIRECTION ( 'NONE',  ( 0.000000000000000000, 0.000000000000000000, -1.000000000000000000 ) ) ;
#5719 = ORIENTED_EDGE ( 'NONE', *, *, #4748, .F. ) ;
#5720 = CARTESIAN_POINT ( 'NONE',  ( -795.0000000000070486, 70.44548139156158584, -96.78565065507937959 ) ) ;
#5721 = DIRECTION ( 'NONE',  ( -1.000000000000000000, 0.000000000000000000, 0.000000000000000000 ) ) ;
#5722 = CARTESIAN_POINT ( 'NONE',  ( -371.2050310453320776, 59.26189320158484009, -109.6722046579261161 ) ) ;
#5723 = EDGE_CURVE ( 'NONE', #4924, #3987, #9917, .T. ) ;
#5724 = CARTESIAN_POINT ( 'NONE',  ( -823.5047064235060361, 114.4566975831561848, -113.1262384684095537 ) ) ;
#5725 = FACE_BOUND ( 'NONE', #8661, .T. ) ;
#5726 = CARTESIAN_POINT ( 'NONE',  ( -828.8285638327239440, 78.67432280806536937, -89.68077099980398259 ) ) ;
#5727 = ORIENTED_EDGE ( 'NONE', *, *, #2231, .F. ) ;
#5728 = CARTESIAN_POINT ( 'NONE',  ( 0.000000000000000000, 24.00000000000001776, -89.68077099980384048 ) ) ;
#5729 = CARTESIAN_POINT ( 'NONE',  ( -374.3412718121057310, 92.91798692285432537, -107.8362180080072363 ) ) ;
#5730 = ORIENTED_EDGE ( 'NONE', *, *, #3720, .T. ) ;
#5731 = CARTESIAN_POINT ( 'NONE',  ( -951.9057582426089539, 113.9552214607315364, -103.3307627799633082 ) ) ;
#5732 = B_SPLINE_CURVE_WITH_KNOTS ( 'NONE', 3,
 ( #10576, #5577, #9350, #7496, #1875, #9468, #6684, #4721, #12201, #1933, #5696, #3721, #1769, #3862, #19, #2619, #2686, #5593, #5462, #4680, #11095, #12215, #4738, #3739, #1951, #6459, #779, #8328, #9304, #5529, #1892, #7753, #8626, #7694, #5084, #10477, #2134, #2074 ),
 .UNSPECIFIED., .F., .F.,
 ( 4, 2, 2, 2, 2, 2, 2, 2, 2, 2, 2, 2, 2, 2, 2, 2, 2, 2, 4 ),
 ( 0.01596000347429179719, 0.01693787742768236571, 0.01791575138107293769, 0.01840468835776813694, 0.01889362533446333967, 0.01987149928785374858, 0.02084937324124415403, 0.02182724719463455948, 0.02280512114802496493, 0.02378299510141537038, 0.02476086905480577582, 0.02573874300819618474, 0.02671661696158659019, 0.02720555393828179291, 0.02769449091497699564, 0.02867236486836743231, 0.02965023882175786898, 0.03062811277514830566, 0.03160598672853873886 ),
 .UNSPECIFIED. ) ;
#5733 = CARTESIAN_POINT ( 'NONE',  ( 1.479627290717497352E-14, -6.000000000000000000, 118.9213562373094817 ) ) ;
#5734 = CARTESIAN_POINT ( 'NONE',  ( -1060.846413679901389, 110.5345601522218146, -136.2353035311979852 ) ) ;
#5735 = PLANE ( 'NONE',  #7666 ) ;
#5736 = CARTESIAN_POINT ( 'NONE',  ( -232.4999999999999716, -9.213203435596478030, -126.4213562373078190 ) ) ;
#5737 = EDGE_LOOP ( 'NONE', ( #471, #5448 ) ) ;
#5738 = CARTESIAN_POINT ( 'NONE',  ( -150.0000000000000000, 139.9999999999999716, -126.4213562373084301 ) ) ;
#5739 = DIRECTION ( 'NONE',  ( 0.000000000000000000, -0.000000000000000000, -1.000000000000000000 ) ) ;
#5740 = CARTESIAN_POINT ( 'NONE',  ( -795.0000000000021600, 107.1049510380564129, -141.4553492942762318 ) ) ;
#5741 = B_SPLINE_CURVE_WITH_KNOTS ( 'NONE', 3,
 ( #6227, #9990, #10051, #4559, #655, #3421, #1582, #4368 ),
 .UNSPECIFIED., .F., .F.,
 ( 4, 2, 2, 4 ),
 ( 0.005257893453559881088, 0.006567392922673219099, 0.007876892391786557979, 0.01049589133001323227 ),
 .UNSPECIFIED. ) ;
#5742 = DIRECTION ( 'NONE',  ( 3.061276722312011504E-17, -1.000000000000000000, -0.000000000000000000 ) ) ;
#5743 = CARTESIAN_POINT ( 'NONE',  ( 141.4213562373095101, -492.9999999999998863, -1.508194112741312283E-14 ) ) ;
#5744 =( LENGTH_UNIT ( ) NAMED_UNIT ( * ) SI_UNIT ( .MILLI., .METRE. ) );
#5745 = ORIENTED_EDGE ( 'NONE', *, *, #47, .F. ) ;
#5746 = CARTESIAN_POINT ( 'NONE',  ( -373.7480576296653112, 95.20073465036217897, -150.6300429098349980 ) ) ;
#5747 = CARTESIAN_POINT ( 'NONE',  ( -1046.095701327183860, 109.2451008237763546, -141.4553492942764308 ) ) ;
#5748 = CYLINDRICAL_SURFACE ( 'NONE', #5575, 70.00000000000002842 ) ;
#5749 = ORIENTED_EDGE ( 'NONE', *, *, #8881, .T. ) ;
#5750 = ORIENTED_EDGE ( 'NONE', *, *, #5247, .F. ) ;
#5751 = CARTESIAN_POINT ( 'NONE',  ( 19.89219543117309286, 179.2566526312703843, -122.6057988080468277 ) ) ;
#5752 = EDGE_CURVE ( 'NONE', #11517, #2061, #8361, .T. ) ;
#5753 = FACE_BOUND ( 'NONE', #9239, .T. ) ;
#5754 = CARTESIAN_POINT ( 'NONE',  ( -1062.665377791219498, 57.01990411978283646, -146.0307792196448702 ) ) ;
#5755 = CARTESIAN_POINT ( 'NONE',  ( -374.8433861704153855, 76.31617881061603725, -143.8923350075967278 ) ) ;
#5756 = EDGE_CURVE ( 'NONE', #7589, #5668, #11338, .T. ) ;
#5757 = CARTESIAN_POINT ( 'NONE',  ( 9.796085511398436814E-16, 152.0000000000000000, -126.4213562373094959 ) ) ;
#5758 = CARTESIAN_POINT ( 'NONE',  ( -374.1800622106637775, 69.98049622810512460, -108.6123104269852035 ) ) ;
#5759 = FILL_AREA_STYLE_COLOUR ( '', #1341 ) ;
#5760 = FACE_OUTER_BOUND ( 'NONE', #2705, .T. ) ;
#5761 = AXIS2_PLACEMENT_3D ( 'NONE', #11982, #3373, #10929 ) ;
#5762 = EDGE_LOOP ( 'NONE', ( #10342, #4459, #3777, #1288 ) ) ;
#5763 = CIRCLE ( 'NONE', #423, 1.499999999999996447 ) ;
#5764 = CARTESIAN_POINT ( 'NONE',  ( -1057.036663358159558, 58.23757105449750071, -99.57582448894497418 ) ) ;
#5765 = CARTESIAN_POINT ( 'NONE',  ( -1065.000000000006366, 82.00000000000036948, -124.6807709998044231 ) ) ;
#5766 = CARTESIAN_POINT ( 'NONE',  ( 0.000000000000000000, -494.9999999999998863, -126.4213562373094959 ) ) ;
#5767 = ADVANCED_FACE ( 'NONE', ( #1152 ), #8802, .F. ) ;
#5768 = EDGE_LOOP ( 'NONE', ( #9987, #7141, #8117, #8990 ) ) ;
#5769 = CARTESIAN_POINT ( 'NONE',  ( -384.4631009414320033, 88.19375710871752005, -105.6549207029757582 ) ) ;
#5770 = CARTESIAN_POINT ( 'NONE',  ( -126.4213562373094959, -492.9999999999998863, 7.500000000000035527 ) ) ;
#5771 = AXIS2_PLACEMENT_3D ( 'NONE', #4351, #3660, #10090 ) ;
#5772 = ORIENTED_EDGE ( 'NONE', *, *, #5015, .F. ) ;
#5773 = APPLICATION_PROTOCOL_DEFINITION ( 'draft international standard', 'automotive_design', 1998, #6531 ) ;
#5774 = VERTEX_POINT ( 'NONE', #7635 ) ;
#5775 = CARTESIAN_POINT ( 'NONE',  ( -1025.943122242217214, 53.12767954719360830, -118.7903414690682524 ) ) ;
#5776 = EDGE_CURVE ( 'NONE', #9127, #8918, #3664, .T. ) ;
#5777 = DIRECTION ( 'NONE',  ( -1.000000000000000000, 0.000000000000000000, 0.000000000000000000 ) ) ;
#5778 = CARTESIAN_POINT ( 'NONE',  ( -1046.095701327177267, 109.2451008237761982, -107.9061927053324439 ) ) ;
#5779 = DIRECTION ( 'NONE',  ( -0.000000000000000000, -1.000000000000000000, -1.757987137413040192E-14 ) ) ;
#5780 = VERTEX_POINT ( 'NONE', #7939 ) ;
#5781 = EDGE_CURVE ( 'NONE', #5971, #11527, #8119, .T. ) ;
#5782 = CIRCLE ( 'NONE', #7374, 7.500000000000007105 ) ;
#5783 = EDGE_CURVE ( 'NONE', #7247, #3434, #2311, .T. ) ;
#5784 = ORIENTED_EDGE ( 'NONE', *, *, #11852, .T. ) ;
#5785 = CARTESIAN_POINT ( 'NONE',  ( -823.5047064235060361, 114.4566975831561848, -113.1262384684095537 ) ) ;
#5786 = CARTESIAN_POINT ( 'NONE',  ( -1017.963927524549604, 117.4283576114808625, -136.2353035311979284 ) ) ;
#5787 = CARTESIAN_POINT ( 'NONE',  ( -30.00000000000000000, -6.000000000000000000, -30.00000000000000000 ) ) ;
#5788 = ADVANCED_FACE ( 'NONE', ( #3171 ), #9094, .F. ) ;
#5789 = CIRCLE ( 'NONE', #11910, 7.500000000000007105 ) ;
#5790 = AXIS2_PLACEMENT_3D ( 'NONE', #5757, #9533, #1078 ) ;
#5791 = CARTESIAN_POINT ( 'NONE',  ( -926.5138833012644000, 125.7648744980332225, -122.7172756069789159 ) ) ;
#5792 = ORIENTED_EDGE ( 'NONE', *, *, #3282, .T. ) ;
#5793 = CARTESIAN_POINT ( 'NONE',  ( -951.4198147059589701, 125.0824040815807194, -124.6807709998040252 ) ) ;
#5794 = CARTESIAN_POINT ( 'NONE',  ( 1.387778780781445676E-14, -6.000000000000000000, 126.4213562373094959 ) ) ;
#5795 = DIRECTION ( 'NONE',  ( 0.000000000000000000, 0.000000000000000000, 1.000000000000000000 ) ) ;
#5796 = CARTESIAN_POINT ( 'NONE',  ( -853.1108559448500728, 99.60875591605696400, -149.7857175106632610 ) ) ;
#5797 = ADVANCED_FACE ( 'NONE', ( #1502 ), #7125, .F. ) ;
#5798 = CARTESIAN_POINT ( 'NONE',  ( -52.49999999999999289, 139.9999999999999716, -126.4213562373090696 ) ) ;
#5799 = DIRECTION ( 'NONE',  ( -1.000000000000000000, 0.000000000000000000, 0.000000000000000000 ) ) ;
#5800 = CYLINDRICAL_SURFACE ( 'NONE', #5811, 7.500000000000007105 ) ;
#5801 = EDGE_LOOP ( 'NONE', ( #785, #5727 ) ) ;
#5802 = VECTOR ( 'NONE', #5242, 1000.000000000000000 ) ;
#5803 = AXIS2_PLACEMENT_3D ( 'NONE', #6555, #115, #6675 ) ;
#5804 = AXIS2_PLACEMENT_3D ( 'NONE', #5907, #2086, #330 ) ;
#5805 = DIRECTION ( 'NONE',  ( 3.061276722312011504E-17, -1.000000000000000000, -0.000000000000000000 ) ) ;
#5806 = CARTESIAN_POINT ( 'NONE',  ( -974.6181169426273527, 104.3135445892218200, -149.7857175106634884 ) ) ;
#5807 = CARTESIAN_POINT ( 'NONE',  ( -305.0000000000000568, 81.99999999999995737, -159.6807709998038547 ) ) ;
#5808 = ORIENTED_EDGE ( 'NONE', *, *, #6542, .T. ) ;
#5809 = VERTEX_POINT ( 'NONE', #433 ) ;
#5810 = CARTESIAN_POINT ( 'NONE',  ( 1.250503886288004501E-12, -6.000000000000004441, -13.92135623730950478 ) ) ;
#5811 = AXIS2_PLACEMENT_3D ( 'NONE', #997, #54, #4763 ) ;
#5812 = CARTESIAN_POINT ( 'NONE',  ( -818.8614508132119454, 78.01542073698772128, -105.0789755614320029 ) ) ;
#5813 = FACE_BOUND ( 'NONE', #10553, .T. ) ;
#5814 = CARTESIAN_POINT ( 'NONE',  ( -818.1708872189602744, 40.82851623284160070, -146.0307792196448702 ) ) ;
#5815 = ORIENTED_EDGE ( 'NONE', *, *, #1407, .T. ) ;
#5816 = CARTESIAN_POINT ( 'NONE',  ( -374.9580429156226842, 78.77578507266967733, -144.4605282461973275 ) ) ;
#5817 = CARTESIAN_POINT ( 'NONE',  ( -141.4213562373095101, -494.9999999999998863, 3.644282033693712520E-14 ) ) ;
#5818 = CARTESIAN_POINT ( 'NONE',  ( -382.6913354005332621, 69.27723932749148616, -109.2458039676438091 ) ) ;
#5819 = DIRECTION ( 'NONE',  ( 1.000000000000000000, -1.026341648675396322E-47, 2.081668171172161734E-17 ) ) ;
#5820 = ORIENTED_EDGE ( 'NONE', *, *, #10228, .F. ) ;
#5821 = CIRCLE ( 'NONE', #9380, 7.500000000000007105 ) ;
#5822 = VECTOR ( 'NONE', #4994, 1000.000000000000000 ) ;
#5823 = DIRECTION ( 'NONE',  ( -0.000000000000000000, 1.000000000000000000, -0.000000000000000000 ) ) ;
#5824 = EDGE_LOOP ( 'NONE', ( #8490, #8112, #8416, #12092 ) ) ;
#5825 = ORIENTED_EDGE ( 'NONE', *, *, #5543, .F. ) ;
#5826 = CARTESIAN_POINT ( 'NONE',  ( -8.500000000000003553, 25.00000000000002132, -126.4213562373094959 ) ) ;
#5827 = CARTESIAN_POINT ( 'NONE',  ( -1065.000000000002501, 60.65002596136933732, -103.3307627799636350 ) ) ;
#5828 = CARTESIAN_POINT ( 'NONE',  ( -795.0000000000043201, 62.00000000000031974, -124.6807709998041815 ) ) ;
#5829 = CARTESIAN_POINT ( 'NONE',  ( -854.0803342822151762, 23.97549884981696167, -130.5712005305403238 ) ) ;
#5830 = VERTEX_POINT ( 'NONE', #4292 ) ;
#5831 = LINE ( 'NONE', #10654, #11552 ) ;
#5832 = VECTOR ( 'NONE', #6001, 1000.000000000000000 ) ;
#5833 = CARTESIAN_POINT ( 'NONE',  ( -382.8521778068924277, 69.69159708733664615, -108.8740338450474923 ) ) ;
#5834 = VERTEX_POINT ( 'NONE', #4223 ) ;
#5835 = DIRECTION ( 'NONE',  ( 0.000000000000000000, 1.000000000000000000, 0.000000000000000000 ) ) ;
#5836 = ORIENTED_EDGE ( 'NONE', *, *, #6479, .F. ) ;
#5837 = ORIENTED_EDGE ( 'NONE', *, *, #2907, .F. ) ;
#5838 = CARTESIAN_POINT ( 'NONE',  ( -928.4218612484631876, 59.99049470396640515, -118.7903414690680535 ) ) ;
#5839 = ADVANCED_FACE ( 'NONE', ( #6263 ), #2815, .T. ) ;
#5840 = DIRECTION ( 'NONE',  ( -0.000000000000000000, 1.000000000000000000, -0.000000000000000000 ) ) ;
#5841 = DIRECTION ( 'NONE',  ( -8.163404592832030268E-17, 1.000000000000000000, -0.000000000000000000 ) ) ;
#5842 = EDGE_CURVE ( 'NONE', #4282, #6950, #11107, .T. ) ;
#5843 = VECTOR ( 'NONE', #5887, 1000.000000000000000 ) ;
#5844 = CARTESIAN_POINT ( 'NONE',  ( -1065.000000000000455, 107.1049510380560719, -107.9061927053323302 ) ) ;
#5845 = DIRECTION ( 'NONE',  ( -0.000000000000000000, 1.000000000000000000, 1.669238443041288415E-16 ) ) ;
#5846 = EDGE_CURVE ( 'NONE', #9416, #822, #10775, .T. ) ;
#5847 = EDGE_LOOP ( 'NONE', ( #5423, #240, #1540, #10764 ) ) ;
#5848 = PRODUCT_DEFINITION_SHAPE ( 'NONE', 'NONE',  #12241 ) ;
#5849 = VERTEX_POINT ( 'NONE', #7061 ) ;
#5850 = CARTESIAN_POINT ( 'NONE',  ( -926.9570750291553622, 111.1083136274928620, -99.57582448894491733 ) ) ;
#5851 = CIRCLE ( 'NONE', #4484, 7.500000000000007105 ) ;
#5852 = EDGE_CURVE ( 'NONE', #7207, #1622, #1055, .T. ) ;
#5853 = ADVANCED_FACE ( 'NONE', ( #9969 ), #6138, .F. ) ;
#5854 = CARTESIAN_POINT ( 'NONE',  ( -1030.931480980267906, 117.9615145441170654, -124.6807709998043521 ) ) ;
#5855 = ORIENTED_EDGE ( 'NONE', *, *, #10682, .F. ) ;
#5856 = VECTOR ( 'NONE', #2888, 1000.000000000000000 ) ;
#5857 = DIRECTION ( 'NONE',  ( -2.081668171172161734E-17, -4.930380657631308019E-31, 1.000000000000000000 ) ) ;
#5858 = LINE ( 'NONE', #6788, #10441 ) ;
#5859 = CARTESIAN_POINT ( 'NONE',  ( -974.4564103291385209, 111.0951925441807759, -146.0307792196441312 ) ) ;
#5860 = CARTESIAN_POINT ( 'NONE',  ( -372.9463709484128913, 100.0680782940595748, -116.0142139199710130 ) ) ;
#5861 = PRODUCT_RELATED_PRODUCT_CATEGORY ( 'part', '', ( #6734 ) ) ;
#5862 = CARTESIAN_POINT ( 'NONE',  ( -3.161662739628749519E-15, 267.2792206135785591, -126.4213562373094959 ) ) ;
#5863 = DIRECTION ( 'NONE',  ( 1.000000000000000000, 0.000000000000000000, 0.000000000000000000 ) ) ;
#5864 =( NAMED_UNIT ( * ) PLANE_ANGLE_UNIT ( ) SI_UNIT ( $, .RADIAN. ) );
#5865 = ORIENTED_EDGE ( 'NONE', *, *, #6817, .F. ) ;
#5866 = CYLINDRICAL_SURFACE ( 'NONE', #7168, 69.99999999999995737 ) ;
#5867 = CARTESIAN_POINT ( 'NONE',  ( -1046.261572611719657, 104.4651992465226868, -146.0307792196445575 ) ) ;
#5868 = VECTOR ( 'NONE', #6235, 1000.000000000000000 ) ;
#5869 = AXIS2_PLACEMENT_3D ( 'NONE', #3284, #10710, #1321 ) ;
#5870 = FACE_BOUND ( 'NONE', #5580, .T. ) ;
#5871 = ORIENTED_EDGE ( 'NONE', *, *, #4795, .F. ) ;
#5872 = EDGE_CURVE ( 'NONE', #11388, #8092, #3345, .T. ) ;
#5873 = ORIENTED_EDGE ( 'NONE', *, *, #10530, .F. ) ;
#5874 = PLANE ( 'NONE',  #9952 ) ;
#5875 = CARTESIAN_POINT ( 'NONE',  ( -1027.375436305353333, 71.63039521860234515, -152.5758913445296230 ) ) ;
#5876 = VERTEX_POINT ( 'NONE', #10031 ) ;
#5877 =( GEOMETRIC_REPRESENTATION_CONTEXT ( 3 ) GLOBAL_UNCERTAINTY_ASSIGNED_CONTEXT ( ( #5967 ) ) GLOBAL_UNIT_ASSIGNED_CONTEXT ( ( #8733, #7049, #375 ) ) REPRESENTATION_CONTEXT ( 'NONE', 'WORKASPACE' ) );
#5878 = CARTESIAN_POINT ( 'NONE',  ( -383.7345387547151745, 72.53406450605939426, -142.3107974752694531 ) ) ;
#5879 = DIRECTION ( 'NONE',  ( 0.000000000000000000, -1.000000000000000000, 0.000000000000000000 ) ) ;
#5880 = CARTESIAN_POINT ( 'NONE',  ( -374.9733877151688262, 79.55905688470338077, -104.8208928575475767 ) ) ;
#5881 = CARTESIAN_POINT ( 'NONE',  ( 9.184850993605161750E-16, -494.9999999999998863, -133.9213562373095101 ) ) ;
#5882 = DIRECTION ( 'NONE',  ( 0.000000000000000000, 0.000000000000000000, 1.000000000000000000 ) ) ;
#5883 = ORIENTED_EDGE ( 'NONE', *, *, #4216, .F. ) ;
#5884 = AXIS2_PLACEMENT_3D ( 'NONE', #3027, #11728, #10732 ) ;
#5885 = VECTOR ( 'NONE', #5355, 1000.000000000000000 ) ;
#5886 = ORIENTED_EDGE ( 'NONE', *, *, #355, .F. ) ;
#5887 = DIRECTION ( 'NONE',  ( -0.000000000000000000, 1.000000000000000000, 7.930164461608263644E-17 ) ) ;
#5888 = CARTESIAN_POINT ( 'NONE',  ( 20.00183334024216464, 177.6837603104920618, -124.8316880602247068 ) ) ;
#5889 = CARTESIAN_POINT ( 'NONE',  ( -1032.589060384100776, 47.36392975189028931, -113.1262384684095537 ) ) ;
#5890 = CARTESIAN_POINT ( 'NONE',  ( -828.5765974139392256, 80.27527354417625816, -104.7529721962251585 ) ) ;
#5891 = DIRECTION ( 'NONE',  ( 0.000000000000000000, 0.000000000000000000, 1.000000000000000000 ) ) ;
#5892 = CARTESIAN_POINT ( 'NONE',  ( -1025.806732200655688, 55.05754055295027172, -136.2353035311988663 ) ) ;
#5893 = VERTEX_POINT ( 'NONE', #5086 ) ;
#5894 = APPLICATION_CONTEXT ( 'automotive_design' ) ;
#5895 = DIRECTION ( 'NONE',  ( -6.195440985631455317E-17, 0.000000000000000000, 1.000000000000000000 ) ) ;
#5896 = AXIS2_PLACEMENT_3D ( 'NONE', #742, #4520, #2846 ) ;
#5897 = CARTESIAN_POINT ( 'NONE',  ( -384.9908864334298642, 81.14062117122209372, -104.6969719710837268 ) ) ;
#5898 = ORIENTED_EDGE ( 'NONE', *, *, #5781, .F. ) ;
#5899 = PLANE ( 'NONE',  #2080 ) ;
#5900 = VERTEX_POINT ( 'NONE', #384 ) ;
#5901 = AXIS2_PLACEMENT_3D ( 'NONE', #56, #10449, #10925 ) ;
#5902 = FACE_OUTER_BOUND ( 'NONE', #7513, .T. ) ;
#5903 = APPLICATION_PROTOCOL_DEFINITION ( 'draft international standard', 'automotive_design', 1998, #1716 ) ;
#5904 = EDGE_LOOP ( 'NONE', ( #6825, #7169 ) ) ;
#5905 = CARTESIAN_POINT ( 'NONE',  ( -901.9718911164643487, 59.00785292138902349, -113.1262384684096105 ) ) ;
#5906 = CARTESIAN_POINT ( 'NONE',  ( 0.01885174614367843282, 0.8831628875414415658, -9.000000000000001776 ) ) ;
#5907 = CARTESIAN_POINT ( 'NONE',  ( -89.99999999999998579, -9.213203435596451385, -126.4213562373088564 ) ) ;
#5908 = AXIS2_PLACEMENT_3D ( 'NONE', #171, #7720, #11495 ) ;
#5909 = CARTESIAN_POINT ( 'NONE',  ( -1025.595388641369482, 103.7168792382126128, -99.57582448894517313 ) ) ;
#5910 = FACE_BOUND ( 'NONE', #4102, .T. ) ;
#5911 = CARTESIAN_POINT ( 'NONE',  ( -19.89477560825904234, 178.6155358530109538, -126.7324661926051448 ) ) ;
#5912 = EDGE_CURVE ( 'NONE', #4307, #10145, #4391, .T. ) ;
#5913 = ORIENTED_EDGE ( 'NONE', *, *, #4058, .F. ) ;
#5914 = CARTESIAN_POINT ( 'NONE',  ( -374.9931058222078377, 80.86295360366069929, -154.6597799724412710 ) ) ;
#5915 = EDGE_CURVE ( 'NONE', #9416, #4019, #1627, .T. ) ;
#5916 = AXIS2_PLACEMENT_3D ( 'NONE', #4857, #7581, #3873 ) ;
#5917 = ORIENTED_EDGE ( 'NONE', *, *, #9611, .T. ) ;
#5918 = CARTESIAN_POINT ( 'NONE',  ( -1014.911393615048723, 99.73439156314999821, -96.78565065507932275 ) ) ;
#5919 = VERTEX_POINT ( 'NONE', #7378 ) ;
#5920 = CARTESIAN_POINT ( 'NONE',  ( -22.49999999999997868, -9.213203435596451385, -126.4213562373092685 ) ) ;
#5921 = CARTESIAN_POINT ( 'NONE',  ( -112.4999999999999716, 24.00000000000001421, -126.4213562373086575 ) ) ;
#5922 = CARTESIAN_POINT ( 'NONE',  ( -991.5701548301638013, 122.8678427087060214, -122.7172756069787170 ) ) ;
#5923 = VERTEX_POINT ( 'NONE', #10280 ) ;
#5924 = CARTESIAN_POINT ( 'NONE',  ( 7.500000000000000000, -5.196152422706605378, 8.999999999999998224 ) ) ;
#5925 = CARTESIAN_POINT ( 'NONE',  ( -818.8285638327205334, 79.00074005404771071, -104.9041682110412239 ) ) ;
#5926 = FACE_OUTER_BOUND ( 'NONE', #4011, .T. ) ;
#5927 = CARTESIAN_POINT ( 'NONE',  ( -1054.691024341075263, 108.1159421897237962, -141.4553492942763739 ) ) ;
#5928 = FILL_AREA_STYLE_COLOUR ( '', #9661 ) ;
#5929 = DIRECTION ( 'NONE',  ( 3.061276722312011504E-17, -1.000000000000000000, 0.000000000000000000 ) ) ;
#5930 = SHAPE_REPRESENTATION_RELATIONSHIP ( 'NONE' , 'NONE' ,  #12068, #9120 ) ;
#5931 = ORIENTED_EDGE ( 'NONE', *, *, #5643, .T. ) ;
#5932 = CYLINDRICAL_SURFACE ( 'NONE', #8048, 7.500000000000012434 ) ;
#5933 = ADVANCED_FACE ( 'NONE', ( #3527 ), #12008, .F. ) ;
#5934 = CARTESIAN_POINT ( 'NONE',  ( 1.875296586882326249E-12, 12.00000000000000000, 46.07864376269049700 ) ) ;
#5935 = CARTESIAN_POINT ( 'NONE',  ( -1054.913455627173789, 103.6024512377076974, -146.0307792196445291 ) ) ;
#5936 = B_SPLINE_CURVE_WITH_KNOTS ( 'NONE', 3,
 ( #2748, #3531, #4481, #1763, #8255, #3733, #3595, #3668 ),
 .UNSPECIFIED., .F., .F.,
 ( 4, 2, 2, 4 ),
 ( 0.01498083277331294615, 0.01629713195395221526, 0.01761343113459148610, 0.02024602949587002432 ),
 .UNSPECIFIED. ) ;
#5937 = CARTESIAN_POINT ( 'NONE',  ( 1.562900236585165577E-12, -6.000000000000004441, 16.07864376269049700 ) ) ;
#5938 = ORIENTED_EDGE ( 'NONE', *, *, #7308, .F. ) ;
#5939 = EDGE_LOOP ( 'NONE', ( #10719, #387 ) ) ;
#5940 = CARTESIAN_POINT ( 'NONE',  ( 35.00000000000000000, 152.0000000000000000, -89.68077099980384048 ) ) ;
#5941 = CARTESIAN_POINT ( 'NONE',  ( -1056.743458481019616, 64.45745743522664384, -152.5758913445293956 ) ) ;
#5942 = CARTESIAN_POINT ( 'NONE',  ( -819.3325619471245318, 76.46264315494626373, -143.9014485902362708 ) ) ;
#5943 = DIRECTION ( 'NONE',  ( -0.000000000000000000, -1.000000000000000000, -0.000000000000000000 ) ) ;
#5944 = CYLINDRICAL_SURFACE ( 'NONE', #10344, 7.500000000000007105 ) ;
#5945 = CARTESIAN_POINT ( 'NONE',  ( -373.4675643629642536, 66.11521760855615071, -112.3653755622224111 ) ) ;
#5946 = EDGE_CURVE ( 'NONE', #9851, #20, #5178, .T. ) ;
#5948 = EDGE_CURVE ( 'NONE', #3434, #8433, #8179, .T. ) ;
#5947 =( NAMED_UNIT ( * ) SI_UNIT ( $, .STERADIAN. ) SOLID_ANGLE_UNIT ( ) );
#5949 = ORIENTED_EDGE ( 'NONE', *, *, #9412, .T. ) ;
#5950 = FACE_OUTER_BOUND ( 'NONE', #4266, .T. ) ;
#5951 = VERTEX_POINT ( 'NONE', #11017 ) ;
#5952 = PRODUCT_DEFINITION_SHAPE ( 'NONE', 'NONE',  #12250 ) ;
#5953 = ORIENTED_EDGE ( 'NONE', *, *, #9540, .T. ) ;
#5954 = CARTESIAN_POINT ( 'NONE',  ( -1048.417899310738221, 40.17786091688638095, -118.7903414690680250 ) ) ;
#5955 = CARTESIAN_POINT ( 'NONE',  ( 1.414009460465297036E-14, -9.213203435596451385, -126.4213562373094959 ) ) ;
#5956 = CARTESIAN_POINT ( 'NONE',  ( -20.00000000000000000, 182.6968134406616002, -124.6807709998189466 ) ) ;
#5957 = CARTESIAN_POINT ( 'NONE',  ( -817.2011019090375612, 28.13185037056175375, -130.5712005305403238 ) ) ;
#5958 = ORIENTED_EDGE ( 'NONE', *, *, #5002, .F. ) ;
#5959 = ORIENTED_EDGE ( 'NONE', *, *, #7571, .F. ) ;
#5960 = DIRECTION ( 'NONE',  ( 0.000000000000000000, 1.000000000000000000, -0.000000000000000000 ) ) ;
#5961 = ORIENTED_EDGE ( 'NONE', *, *, #121, .T. ) ;
#5962 = PRODUCT_CONTEXT ( 'NONE', #426, 'mechanical' ) ;
#5963 = ORIENTED_EDGE ( 'NONE', *, *, #10066, .F. ) ;
#5964 = AXIS2_PLACEMENT_3D ( 'NONE', #8222, #9197, #5235 ) ;
#5965 = CARTESIAN_POINT ( 'NONE',  ( -1048.334963668458158, 42.40858384259915681, -113.1262384684096105 ) ) ;
#5966 = CARTESIAN_POINT ( 'NONE',  ( -89.99999999999998579, -9.213203435596451385, -126.4213562373088564 ) ) ;
#5967 = UNCERTAINTY_MEASURE_WITH_UNIT (LENGTH_MEASURE( 1.000000000000000082E-05 ), #8733, 'distance_accuracy_value', 'NONE');
#5968 = CARTESIAN_POINT ( 'NONE',  ( -993.0619804577127070, 103.7129695969639442, -99.57582448894480365 ) ) ;
#5969 = DIRECTION ( 'NONE',  ( 1.486905836551548832E-16, -1.000000000000000000, 0.000000000000000000 ) ) ;
#5970 = AXIS2_PLACEMENT_3D ( 'NONE', #10220, #1757, #6323 ) ;
#5971 = VERTEX_POINT ( 'NONE', #11083 ) ;
#5972 = FACE_OUTER_BOUND ( 'NONE', #11294, .T. ) ;
#5973 =( NAMED_UNIT ( * ) SI_UNIT ( $, .STERADIAN. ) SOLID_ANGLE_UNIT ( ) );
#5974 = ORIENTED_EDGE ( 'NONE', *, *, #8854, .F. ) ;
#5975 = CARTESIAN_POINT ( 'NONE',  ( -853.2189900670988436, 91.12674563889150647, -96.78565065507912379 ) ) ;
#5976 = CARTESIAN_POINT ( 'NONE',  ( -852.8274699693135972, 120.9962006285028906, -130.5712005305406933 ) ) ;
#5977 = CARTESIAN_POINT ( 'NONE',  ( -955.0000000000038654, 62.00000000000029132, -124.6807709998041815 ) ) ;
#5978 = AXIS2_PLACEMENT_3D ( 'NONE', #8552, #7806, #7683 ) ;
#5979 = EDGE_CURVE ( 'NONE', #10717, #6923, #638, .T. ) ;
#5980 = CARTESIAN_POINT ( 'NONE',  ( 19.87365484478755917, 180.4904287905548586, -122.4362480607051253 ) ) ;
#5981 = CARTESIAN_POINT ( 'NONE',  ( -97.50000000000000000, 139.9999999999999716, -126.4213562373088564 ) ) ;
#5982 = CIRCLE ( 'NONE', #1642, 7.500000000000007105 ) ;
#5983 = CARTESIAN_POINT ( 'NONE',  ( 0.000000000000000000, 0.000000000000000000, -118.9213562373094817 ) ) ;
#5984 = DIRECTION ( 'NONE',  ( 0.000000000000000000, 1.000000000000000000, -0.000000000000000000 ) ) ;
#5985 = FACE_OUTER_BOUND ( 'NONE', #9525, .T. ) ;
#5986 = PLANE ( 'NONE',  #10368 ) ;
#5987 = ORIENTED_EDGE ( 'NONE', *, *, #3362, .T. ) ;
#5988 = DIRECTION ( 'NONE',  ( 0.000000000000000000, 0.000000000000000000, -1.000000000000000000 ) ) ;
#5989 = DIRECTION ( 'NONE',  ( -0.000000000000000000, -0.000000000000000000, -1.000000000000000000 ) ) ;
#5990 = LINE ( 'NONE', #363, #4779 ) ;
#5991 = CARTESIAN_POINT ( 'NONE',  ( -951.7027691703365235, 118.7449601027238799, -141.4553492942759192 ) ) ;
#5992 = CIRCLE ( 'NONE', #9943, 69.99999999999998579 ) ;
#5993 = EDGE_CURVE ( 'NONE', #1262, #4924, #8917, .T. ) ;
#5994 = FACE_OUTER_BOUND ( 'NONE', #3138, .T. ) ;
#5995 = ADVANCED_FACE ( 'NONE', ( #2549 ), #10339, .T. ) ;
#5996 = ORIENTED_EDGE ( 'NONE', *, *, #8202, .F. ) ;
#5997 = ORIENTED_EDGE ( 'NONE', *, *, #7440, .T. ) ;
#5998 = CARTESIAN_POINT ( 'NONE',  ( 19.87298152431207399, 180.3898216659918035, -122.4301876295843101 ) ) ;
#5999 = FACE_BOUND ( 'NONE', #4598, .T. ) ;
#6000 = CARTESIAN_POINT ( 'NONE',  ( -1013.120138696094841, 73.26074010992857666, -152.5758913445291682 ) ) ;
#6001 = DIRECTION ( 'NONE',  ( -8.163404592832030268E-17, 1.000000000000000000, -0.000000000000000000 ) ) ;
#6002 = CIRCLE ( 'NONE', #9561, 5.999999999999999112 ) ;
#6003 = EDGE_CURVE ( 'NONE', #1493, #10476, #11887, .T. ) ;
#6004 = AXIS2_PLACEMENT_3D ( 'NONE', #9338, #12192, #9143 ) ;
#6005 = CARTESIAN_POINT ( 'NONE',  ( 0.5595136366745770973, -4.349754824376205420, -9.000000000000001776 ) ) ;
#6006 = CARTESIAN_POINT ( 'NONE',  ( 0.8038475772933637575, -10.39230484541326405, -2.038422702671202938E-16 ) ) ;
#6007 = CARTESIAN_POINT ( 'NONE',  ( -821.3274957761739188, 74.33250986977238028, -94.70253061673973605 ) ) ;
#6008 = FILL_AREA_STYLE ('',( #7929 ) ) ;
#6009 = PLANE ( 'NONE',  #10594 ) ;
#6010 = CARTESIAN_POINT ( 'NONE',  ( -928.3598895238005753, 61.90886769853032945, -136.2353035311983263 ) ) ;
#6011 = EDGE_LOOP ( 'NONE', ( #8110, #5395, #8180, #5442 ) ) ;
#6012 = CIRCLE ( 'NONE', #6795, 7.500000000000007105 ) ;
#6013 = CIRCLE ( 'NONE', #11147, 8.500000000000003553 ) ;
#6014 = EDGE_CURVE ( 'NONE', #1192, #4655, #3592, .T. ) ;
#6015 = CARTESIAN_POINT ( 'NONE',  ( -1057.832023714519210, 42.29985473022490794, -122.7172756069794559 ) ) ;
#6016 = CARTESIAN_POINT ( 'NONE',  ( -19.99999999999999645, 177.7115707886035807, -124.6807709997916334 ) ) ;
#6017 = LINE ( 'NONE', #3343, #2067 ) ;
#6018 = CARTESIAN_POINT ( 'NONE',  ( -1017.027421246632343, 56.01181809833700243, -136.2353035311990368 ) ) ;
#6019 = VERTEX_POINT ( 'NONE', #6383 ) ;
#6020 = DIRECTION ( 'NONE',  ( 0.000000000000000000, 0.000000000000000000, -1.000000000000000000 ) ) ;
#6021 = ORIENTED_EDGE ( 'NONE', *, *, #2927, .F. ) ;
#6022 = CARTESIAN_POINT ( 'NONE',  ( 7.750278301654327992E-16, 197.0000000000000000, -124.6807709998038405 ) ) ;
#6023 = ORIENTED_EDGE ( 'NONE', *, *, #5948, .T. ) ;
#6024 = ADVANCED_FACE ( 'NONE', ( #9161 ), #11273, .F. ) ;
#6025 = ADVANCED_FACE ( 'NONE', ( #8250 ), #697, .F. ) ;
#6026 = AXIS2_PLACEMENT_3D ( 'NONE', #9874, #458, #7025 ) ;
#6027 = VERTEX_POINT ( 'NONE', #768 ) ;
#6028 = CARTESIAN_POINT ( 'NONE',  ( -997.9925905826713688, 37.72784750336357007, -118.7903414690684514 ) ) ;
#6029 = DIRECTION ( 'NONE',  ( 0.000000000000000000, -1.000000000000000000, 0.000000000000000000 ) ) ;
#6030 = CARTESIAN_POINT ( 'NONE',  ( -21.06311735264367613, 179.9260305249855207, -126.4071080971834391 ) ) ;
#6031 = EDGE_CURVE ( 'NONE', #882, #4581, #3588, .T. ) ;
#6032 = CIRCLE ( 'NONE', #5035, 4.000000000000003553 ) ;
#6033 = CARTESIAN_POINT ( 'NONE',  ( -951.9057582426089539, 113.9552214607315364, -103.3307627799633082 ) ) ;
#6034 = LINE ( 'NONE', #3352, #10084 ) ;
#6035 = VERTEX_POINT ( 'NONE', #12078 ) ;
#6036 = CARTESIAN_POINT ( 'NONE',  ( 1.240837498110468453E-14, 12.00000000000001776, -126.4213562373094959 ) ) ;
#6037 = VERTEX_POINT ( 'NONE', #6449 ) ;
#6038 = CARTESIAN_POINT ( 'NONE',  ( -795.0000000000079581, 93.55451860843940892, -96.78565065507920906 ) ) ;
#6039 = FACE_OUTER_BOUND ( 'NONE', #10205, .T. ) ;
#6040 = CARTESIAN_POINT ( 'NONE',  ( -852.8175266017517515, 121.6828083272129106, -126.6442663926292624 ) ) ;
#6041 = DIRECTION ( 'NONE',  ( 1.186840563529527301E-16, -1.000000000000000000, 0.000000000000000000 ) ) ;
#6042 = LINE ( 'NONE', #9809, #3991 ) ;
#6043 = ADVANCED_BREP_SHAPE_REPRESENTATION ( '', ( #3982, #11957 ), #10774 ) ;
#6044 = DIRECTION ( 'NONE',  ( 0.000000000000000000, 0.000000000000000000, -1.000000000000000000 ) ) ;
#6045 = DIRECTION ( 'NONE',  ( 0.000000000000000000, 0.000000000000000000, -1.000000000000000000 ) ) ;
#6046 = FACE_BOUND ( 'NONE', #4248, .T. ) ;
#6047 = CARTESIAN_POINT ( 'NONE',  ( -1057.832023714519664, 42.29985473022490794, -124.6807709998044373 ) ) ;
#6048 = CARTESIAN_POINT ( 'NONE',  ( -373.1999217634634078, 99.04079563999313507, -114.1166220202556616 ) ) ;
#6049 = VECTOR ( 'NONE', #6999, 1000.000000000000000 ) ;
#6050 = DIRECTION ( 'NONE',  ( -0.000000000000000000, -1.000000000000000000, -0.000000000000000000 ) ) ;
#6051 = DIRECTION ( 'NONE',  ( 1.000000000000000000, 0.000000000000000000, 0.000000000000000000 ) ) ;
#6052 = ORIENTED_EDGE ( 'NONE', *, *, #7693, .F. ) ;
#6053 = PLANE ( 'NONE',  #5267 ) ;
#6054 = PRODUCT_DEFINITION_SHAPE ( 'NONE', 'NONE',  #11540 ) ;
#6055 = DIRECTION ( 'NONE',  ( 0.000000000000000000, 0.000000000000000000, 1.000000000000000000 ) ) ;
#6056 = DIRECTION ( 'NONE',  ( 0.000000000000000000, 0.000000000000000000, -1.000000000000000000 ) ) ;
#6057 = VECTOR ( 'NONE', #10080, 1000.000000000000000 ) ;
#6058 = ORIENTED_EDGE ( 'NONE', *, *, #5122, .F. ) ;
#6059 = CARTESIAN_POINT ( 'NONE',  ( -384.9016521429225577, 79.29180104530665574, -144.5054763653512850 ) ) ;
#6060 = CARTESIAN_POINT ( 'NONE',  ( -1023.860074334738101, 85.97273905232952984, -154.8742214401228523 ) ) ;
#6061 = CARTESIAN_POINT ( 'NONE',  ( -821.2963138009687327, 74.35985007445715667, -143.1641509997129731 ) ) ;
#6062 = EDGE_CURVE ( 'NONE', #11075, #4285, #7756, .T. ) ;
#6063 = CARTESIAN_POINT ( 'NONE',  ( 0.000000000000000000, 0.000000000000000000, 0.000000000000000000 ) ) ;
#6064 = LINE ( 'NONE', #11868, #8945 ) ;
#6065 = CARTESIAN_POINT ( 'NONE',  ( -370.6647493025599260, 57.74548308484566661, -113.1662857576497174 ) ) ;
#6066 = CARTESIAN_POINT ( 'NONE',  ( -826.3364923082716587, 74.33644497882033875, -94.69033226336712517 ) ) ;
#6067 = ADVANCED_FACE ( 'NONE', ( #12146 ), #11219, .F. ) ;
#6068 = CIRCLE ( 'NONE', #5470, 7.500000000000007105 ) ;
#6069 = FACE_OUTER_BOUND ( 'NONE', #637, .T. ) ;
#6070 = ORIENTED_EDGE ( 'NONE', *, *, #1014, .T. ) ;
#6071 = CARTESIAN_POINT ( 'NONE',  ( -1013.637332661010191, 62.09754518945636903, -146.0307792196449839 ) ) ;
#6072 = VECTOR ( 'NONE', #2586, 1000.000000000000000 ) ;
#6073 = ORIENTED_EDGE ( 'NONE', *, *, #10458, .F. ) ;
#6074 = EDGE_CURVE ( 'NONE', #8540, #11819, #8747, .T. ) ;
#6075 = CARTESIAN_POINT ( 'NONE',  ( 19.99507464840871407, 177.7912328150372332, -124.2124546237747609 ) ) ;
#6076 = VECTOR ( 'NONE', #8848, 1000.000000000000000 ) ;
#6077 = CARTESIAN_POINT ( 'NONE',  ( -1038.708781889661850, 41.03774456592562103, -118.7903414690682240 ) ) ;
#6078 = CARTESIAN_POINT ( 'NONE',  ( -19.88197180057522928, 180.9249649884407631, -122.5105553016253737 ) ) ;
#6079 = ORIENTED_EDGE ( 'NONE', *, *, #1390, .T. ) ;
#6080 = CARTESIAN_POINT ( 'NONE',  ( 141.4213562373095101, 0.000000000000000000, -1.508194112741312283E-14 ) ) ;
#6081 = CARTESIAN_POINT ( 'NONE',  ( -30.00000000000000000, 139.9999999999999716, -126.4213562373092685 ) ) ;
#6082 = ORIENTED_EDGE ( 'NONE', *, *, #1332, .T. ) ;
#6083 = EDGE_CURVE ( 'NONE', #7020, #8838, #8150, .T. ) ;
#6084 = DIRECTION ( 'NONE',  ( -0.000000000000000000, 1.000000000000000000, -0.000000000000000000 ) ) ;
#6085 = ORIENTED_EDGE ( 'NONE', *, *, #10927, .T. ) ;
#6086 = CARTESIAN_POINT ( 'NONE',  ( -854.0902776497797504, 23.28889115110667518, -126.6442663926296603 ) ) ;
#6087 = EDGE_CURVE ( 'NONE', #11020, #5893, #2826, .T. ) ;
#6088 = DIRECTION ( 'NONE',  ( -0.000000000000000000, -1.000000000000000000, -0.000000000000000000 ) ) ;
#6089 = DIRECTION ( 'NONE',  ( 0.000000000000000000, 1.000000000000000000, -0.000000000000000000 ) ) ;
#6090 = PRODUCT_RELATED_PRODUCT_CATEGORY ( 'part', '', ( #118 ) ) ;
#6091 = VECTOR ( 'NONE', #790, 1000.000000000000000 ) ;
#6092 = CARTESIAN_POINT ( 'NONE',  ( -974.7984820115178763, 96.63273410478059589, -96.78565065507896747 ) ) ;
#6093 = CARTESIAN_POINT ( 'NONE',  ( 2.186774452080127126E-12, 0.000000000000000000, 91.07864376269050410 ) ) ;
#6094 = AXIS2_PLACEMENT_3D ( 'NONE', #10138, #5434, #8430 ) ;
#6095 = ORIENTED_EDGE ( 'NONE', *, *, #8925, .F. ) ;
#6096 =( NAMED_UNIT ( * ) PLANE_ANGLE_UNIT ( ) SI_UNIT ( $, .RADIAN. ) );
#6097 = CARTESIAN_POINT ( 'NONE',  ( -384.7907540261165309, 85.90887177978304123, -105.0552917614837867 ) ) ;
#6098 = ORIENTED_EDGE ( 'NONE', *, *, #2172, .F. ) ;
#6099 = DIRECTION ( 'NONE',  ( 0.000000000000000000, 1.000000000000000000, 0.000000000000000000 ) ) ;
#6100 = ORIENTED_EDGE ( 'NONE', *, *, #9825, .F. ) ;
#6101 = CARTESIAN_POINT ( 'NONE',  ( -1065.000000000004093, 93.55451860843899681, -96.78565065507908116 ) ) ;
#6102 = ADVANCED_FACE ( 'NONE', ( #1015 ), #11330, .T. ) ;
#6103 = CIRCLE ( 'NONE', #6884, 7.500000000000007105 ) ;
#6104 = CARTESIAN_POINT ( 'NONE',  ( -926.5289067496701136, 125.3297071905304989, -130.5712005305407786 ) ) ;
#6105 = CARTESIAN_POINT ( 'NONE',  ( 1.250503886288004501E-12, 12.00000000000000000, -13.92135623730950300 ) ) ;
#6106 = CARTESIAN_POINT ( 'NONE',  ( 7.347064133548826625E-16, 139.9999999999999716, -126.4213562373094959 ) ) ;
#6107 = CARTESIAN_POINT ( 'NONE',  ( -1017.963927524554038, 117.4283576114806777, -113.1262384684094968 ) ) ;
#6108 = DIRECTION ( 'NONE',  ( -1.000000000000000000, 0.000000000000000000, 0.000000000000000000 ) ) ;
#6109 = CARTESIAN_POINT ( 'NONE',  ( -818.9567516184583837, 77.53771799247171259, -144.1773011583834716 ) ) ;
#6110 = CIRCLE ( 'NONE', #10839, 7.500000000000007105 ) ;
#6111 = MECHANICAL_DESIGN_GEOMETRIC_PRESENTATION_REPRESENTATION (  '', ( #5118 ), #2363 ) ;
#6112 = DIRECTION ( 'NONE',  ( 0.000000000000000000, 1.000000000000000000, 0.000000000000000000 ) ) ;
#6113 = CARTESIAN_POINT ( 'NONE',  ( 1.387778780781445676E-14, 0.000000000000000000, 126.4213562373094959 ) ) ;
#6114 = AXIS2_PLACEMENT_3D ( 'NONE', #402, #7028, #6108 ) ;
#6115 = CARTESIAN_POINT ( 'NONE',  ( -819.8508737614558868, 81.72136211720568610, -94.97649986144543277 ) ) ;
#6116 = CARTESIAN_POINT ( 'NONE',  ( 7.653191805780027529E-16, 138.9999999999999716, -126.4213562373094959 ) ) ;
#6117 = ORIENTED_EDGE ( 'NONE', *, *, #7730, .T. ) ;
#6118 = FACE_OUTER_BOUND ( 'NONE', #8653, .T. ) ;
#6119 = CARTESIAN_POINT ( 'NONE',  ( -852.8175266017511831, 121.6828083272127685, -124.6807709998041247 ) ) ;
#6120 = DIRECTION ( 'NONE',  ( -1.000000000000000000, 0.000000000000000000, 0.000000000000000000 ) ) ;
#6121 = CARTESIAN_POINT ( 'NONE',  ( -374.9888490819218987, 80.55335064010526480, -94.71470242688155849 ) ) ;
#6122 = CARTESIAN_POINT ( 'NONE',  ( -151.3258811035894098, 12.00000000000000000, -56.13263083939680342 ) ) ;
#6123 = EDGE_LOOP ( 'NONE', ( #1554, #2353 ) ) ;
#6124 = FACE_BOUND ( 'NONE', #9309, .T. ) ;
#6125 = CARTESIAN_POINT ( 'NONE',  ( 0.8038475772933606489, 5.196152422706624918, 8.999999999999998224 ) ) ;
#6126 = CARTESIAN_POINT ( 'NONE',  ( -29.03136272649514638, 180.2041921146316668, -134.6807709998038547 ) ) ;
#6127 = DIRECTION ( 'NONE',  ( 3.061276722312011504E-17, -1.000000000000000000, -0.000000000000000000 ) ) ;
#6128 = CARTESIAN_POINT ( 'NONE',  ( -819.8574495259266541, 75.61847659506229036, -94.68200740722480191 ) ) ;
#6129 = CARTESIAN_POINT ( 'NONE',  ( -818.8285638327206470, 78.67432280806531253, -104.9592124606049879 ) ) ;
#6130 = ORIENTED_EDGE ( 'NONE', *, *, #4346, .T. ) ;
#6131 = CARTESIAN_POINT ( 'NONE',  ( -902.0880155070129831, 62.23309906011792947, -141.4553492942754644 ) ) ;
#6132 = APPLICATION_CONTEXT ( 'automotive_design' ) ;
#6133 = ORIENTED_EDGE ( 'NONE', *, *, #1036, .F. ) ;
#6134 = EDGE_CURVE ( 'NONE', #6278, #4474, #646, .T. ) ;
#6135 = CARTESIAN_POINT ( 'NONE',  ( 19.99903954885881063, 178.7487137633693806, -124.2681297334914632 ) ) ;
#6136 = CARTESIAN_POINT ( 'NONE',  ( -1038.719578313838610, 40.52245044769760085, -122.7172756069793707 ) ) ;
#6137 = ORIENTED_EDGE ( 'NONE', *, *, #8393, .F. ) ;
#6138 = CYLINDRICAL_SURFACE ( 'NONE', #6959, 7.500000000000007105 ) ;
#6139 = ORIENTED_EDGE ( 'NONE', *, *, #5441, .T. ) ;
#6140 = SHAPE_REPRESENTATION ( 'Long Manual Ratchet Lever Handle', ( #11957 ), #4670 ) ;
#6141 = ORIENTED_EDGE ( 'NONE', *, *, #1007, .F. ) ;
#6142 = CARTESIAN_POINT ( 'NONE',  ( -151.3258811035894098, 12.00000000000000000, -56.13263083939680342 ) ) ;
#6143 = CARTESIAN_POINT ( 'NONE',  ( 20.77152989773913916, 180.9696350864299461, -123.5256872951201643 ) ) ;
#6144 = CARTESIAN_POINT ( 'NONE',  ( 0.3563104543936323476, 6.049278984716039531, 7.522341449313131534 ) ) ;
#6145 = ADVANCED_FACE ( 'NONE', ( #248 ), #11310, .F. ) ;
#6146 = CIRCLE ( 'NONE', #6339, 70.00000000000002842 ) ;
#6147 = CARTESIAN_POINT ( 'NONE',  ( -1055.782959745578182, 85.17781532426863578, -95.06748246948041015 ) ) ;
#6148 = DIRECTION ( 'NONE',  ( -0.000000000000000000, -1.000000000000000000, 0.000000000000000000 ) ) ;
#6149 = LINE ( 'NONE', #9916, #3556 ) ;
#6150 = ORIENTED_EDGE ( 'NONE', *, *, #2710, .F. ) ;
#6151 = CARTESIAN_POINT ( 'NONE',  ( -380.0454277744337332, 63.52036806465107333, -117.0044475050485744 ) ) ;
#6152 = CIRCLE ( 'NONE', #7735, 7.500000000000007105 ) ;
#6153 = VERTEX_POINT ( 'NONE', #11390 ) ;
#6154 = DIRECTION ( 'NONE',  ( 0.000000000000000000, -1.000000000000000000, 0.000000000000000000 ) ) ;
#6155 = ORIENTED_EDGE ( 'NONE', *, *, #10410, .F. ) ;
#6156 = CARTESIAN_POINT ( 'NONE',  ( 1.561981751485805177E-12, 163.9999999999999716, 23.57864376269051832 ) ) ;
#6157 = B_SPLINE_CURVE_WITH_KNOTS ( 'NONE', 3,
 ( #3767, #1739, #6359, #10265, #9273, #8358 ),
 .UNSPECIFIED., .F., .F.,
 ( 4, 2, 4 ),
 ( 9.911001995881279201E-05, 0.0005063982416591003089, 0.0009136864633593878935 ),
 .UNSPECIFIED. ) ;
#6158 = CARTESIAN_POINT ( 'NONE',  ( -819.8389179520128209, 63.91331975908082086, -95.06748246948014014 ) ) ;
#6159 = CARTESIAN_POINT ( 'NONE',  ( 19.99707640442948886, 182.6412405632554794, -124.2913783979071951 ) ) ;
#6160 = CARTESIAN_POINT ( 'NONE',  ( -1054.380968608931425, 114.0683136310379524, -124.6807709998043663 ) ) ;
#6161 = CARTESIAN_POINT ( 'NONE',  ( 19.97650381977640066, 180.1919982719466589, -126.1624390054462737 ) ) ;
#6162 = AXIS2_PLACEMENT_3D ( 'NONE', #10288, #9367, #4360 ) ;
#6163 = CARTESIAN_POINT ( 'NONE',  ( 45.53315400109643463, 0.000000000000000000, -230.3419396193597208 ) ) ;
#6164 = TOROIDAL_SURFACE ( 'NONE', #10102, 10.00000000000003730, 1.499999999999998002 ) ;
#6165 = CARTESIAN_POINT ( 'NONE',  ( -60.00000000000000000, 139.9999999999999716, -126.4213562373090696 ) ) ;
#6166 = ADVANCED_FACE ( 'NONE', ( #2871 ), #11576, .T. ) ;
#6167 = DIRECTION ( 'NONE',  ( 0.000000000000000000, 0.000000000000000000, 1.000000000000000000 ) ) ;
#6168 = ADVANCED_FACE ( 'NONE', ( #9595 ), #5944, .F. ) ;
#6169 = CIRCLE ( 'NONE', #4131, 8.999999999999998224 ) ;
#6170 = CARTESIAN_POINT ( 'NONE',  ( -827.1368241426257555, 82.43785830827043526, -104.6842000310832503 ) ) ;
#6171 = DIRECTION ( 'NONE',  ( 0.000000000000000000, 1.000000000000000000, 0.000000000000000000 ) ) ;
#6172 = LINE ( 'NONE', #3088, #2765 ) ;
#6173 = VERTEX_POINT ( 'NONE', #3103 ) ;
#6174 = DIRECTION ( 'NONE',  ( 1.000000000000000000, 0.000000000000000000, 0.000000000000000000 ) ) ;
#6175 = AXIS2_PLACEMENT_3D ( 'NONE', #10152, #1689, #5447 ) ;
#6176 = CARTESIAN_POINT ( 'NONE',  ( -1024.691966601152672, 118.8493250655916142, -124.6807709998039400 ) ) ;
#6177 = EDGE_CURVE ( 'NONE', #4792, #2378, #10465, .T. ) ;
#6178 = DIRECTION ( 'NONE',  ( 0.000000000000000000, 0.000000000000000000, -1.000000000000000000 ) ) ;
#6179 = DIRECTION ( 'NONE',  ( 0.000000000000000000, 0.000000000000000000, 1.000000000000000000 ) ) ;
#6180 = DIRECTION ( 'NONE',  ( -0.000000000000000000, -1.000000000000000000, -1.757987137413040192E-14 ) ) ;
#6181 = VERTEX_POINT ( 'NONE', #71 ) ;
#6182 = ADVANCED_FACE ( 'NONE', ( #6631 ), #3849, .F. ) ;
#6183 = FACE_BOUND ( 'NONE', #6961, .T. ) ;
#6184 = CARTESIAN_POINT ( 'NONE',  ( -902.8257469293334907, 84.21185948885708683, -154.2940595301280950 ) ) ;
#6185 = LINE ( 'NONE', #9951, #2683 ) ;
#6186 = DIRECTION ( 'NONE',  ( -1.000000000000000000, 0.000000000000000000, 0.000000000000000000 ) ) ;
#6187 = LINE ( 'NONE', #9955, #7777 ) ;
#6188 = CARTESIAN_POINT ( 'NONE',  ( -828.6693929326720536, 77.38039550993836713, -94.71761797639442193 ) ) ;
#6189 = AXIS2_PLACEMENT_3D ( 'NONE', #7587, #11482, #3015 ) ;
#6190 = DIRECTION ( 'NONE',  ( -0.05793880415591697725, 0.8576035275428159910, -0.5110374590175372767 ) ) ;
#6191 = VERTEX_POINT ( 'NONE', #3968 ) ;
#6192 = DIRECTION ( 'NONE',  ( 1.000000000000000000, 0.000000000000000000, 0.000000000000000000 ) ) ;
#6193 = CARTESIAN_POINT ( 'NONE',  ( -1048.206790403134164, 45.99070412075050740, -141.4553492942756918 ) ) ;
#6194 = ORIENTED_EDGE ( 'NONE', *, *, #4401, .T. ) ;
#6195 = CIRCLE ( 'NONE', #5390, 7.500000000000007105 ) ;
#6196 = VECTOR ( 'NONE', #6432, 1000.000000000000000 ) ;
#6197 = PLANE ( 'NONE',  #2626 ) ;
#6198 = CARTESIAN_POINT ( 'NONE',  ( -20.77482174596512010, 180.9926187296579201, -123.5402880645762451 ) ) ;
#6199 = ORIENTED_EDGE ( 'NONE', *, *, #4885, .F. ) ;
#6200 = FACE_OUTER_BOUND ( 'NONE', #7017, .T. ) ;
#6201 = CARTESIAN_POINT ( 'NONE',  ( -379.1619848709566440, 102.0000000000000142, -124.6807709998038405 ) ) ;
#6202 = ORIENTED_EDGE ( 'NONE', *, *, #6918, .T. ) ;
#6203 = CARTESIAN_POINT ( 'NONE',  ( -127.5000000000000000, 152.0000000000000000, -126.4213562373086575 ) ) ;
#6204 = ORIENTED_EDGE ( 'NONE', *, *, #9340, .T. ) ;
#6205 = AXIS2_PLACEMENT_3D ( 'NONE', #10248, #2509, #1843 ) ;
#6206 = AXIS2_PLACEMENT_3D ( 'NONE', #6730, #937, #8715 ) ;
#6207 = CIRCLE ( 'NONE', #6408, 7.500000000000007105 ) ;
#6208 = CARTESIAN_POINT ( 'NONE',  ( 7.500000000000000000, 8.082668874372530033E-16, 6.599999999999998757 ) ) ;
#6209 = CARTESIAN_POINT ( 'NONE',  ( -35.00000000000000000, 2.428612866367529932E-14, -159.6807709998040252 ) ) ;
#6210 = CARTESIAN_POINT ( 'NONE',  ( 1.142876642996484321E-14, 24.00000000000001421, -126.4213562373094959 ) ) ;
#6211 = CARTESIAN_POINT ( 'NONE',  ( -1031.794838716553841, 81.34535957697958963, -94.48732055948609343 ) ) ;
#6212 = DIRECTION ( 'NONE',  ( 0.000000000000000000, -1.000000000000000000, 0.000000000000000000 ) ) ;
#6213 = SHAPE_REPRESENTATION ( 'Handle', ( #11957 ), #9978 ) ;
#6214 = CIRCLE ( 'NONE', #7411, 7.500000000000007105 ) ;
#6215 = VERTEX_POINT ( 'NONE', #954 ) ;
#6216 = AXIS2_PLACEMENT_3D ( 'NONE', #4392, #9145, #8165 ) ;
#6217 = CARTESIAN_POINT ( 'NONE',  ( 7.750278301654327006E-16, 197.0000000000000000, -124.6807709998038405 ) ) ;
#6218 = ORIENTED_EDGE ( 'NONE', *, *, #913, .T. ) ;
#6219 = CARTESIAN_POINT ( 'NONE',  ( -20.89767086227280757, 178.8455056537755183, -124.1343435470157743 ) ) ;
#6220 = EDGE_CURVE ( 'NONE', #5193, #7316, #4725, .T. ) ;
#6221 =( NAMED_UNIT ( * ) PLANE_ANGLE_UNIT ( ) SI_UNIT ( $, .RADIAN. ) );
#6222 = CARTESIAN_POINT ( 'NONE',  ( -180.0000000000000000, 151.9999999999999716, -126.4213562373082453 ) ) ;
#6223 = VERTEX_POINT ( 'NONE', #4891 ) ;
#6224 = CARTESIAN_POINT ( 'NONE',  ( -827.8051113588386443, 81.72309053119306554, -154.3319006730158094 ) ) ;
#6226 = EDGE_CURVE ( 'NONE', #5315, #8861, #10148, .T. ) ;
#6225 = CARTESIAN_POINT ( 'NONE',  ( -953.2897746444517679, 79.65961628290871488, -95.06748246948048120 ) ) ;
#6227 = CARTESIAN_POINT ( 'NONE',  ( 0.000000000000000000, 7.794228634059941818, 4.500000000000007994 ) ) ;
#6228 = CARTESIAN_POINT ( 'NONE',  ( -21.06614900906485488, 180.8501015263614704, -126.2877667442240153 ) ) ;
#6229 = EDGE_CURVE ( 'NONE', #4655, #1192, #451, .T. ) ;
#6230 = LINE ( 'NONE', #11244, #3337 ) ;
#6231 = CARTESIAN_POINT ( 'NONE',  ( -820.0477536417059810, 75.38653579115350567, -143.5572547269224515 ) ) ;
#6232 = CARTESIAN_POINT ( 'NONE',  ( 0.000000000000000000, 12.00000000000000000, -89.68077099980401101 ) ) ;
#6233 = CARTESIAN_POINT ( 'NONE',  ( -379.4351561318256358, 62.45525130393783542, -120.2966889111102660 ) ) ;
#6234 = ORIENTED_EDGE ( 'NONE', *, *, #10821, .F. ) ;
#6235 = DIRECTION ( 'NONE',  ( -0.000000000000000000, -1.000000000000000000, -0.000000000000000000 ) ) ;
#6236 = CARTESIAN_POINT ( 'NONE',  ( -904.2101318205999405, 125.2895275102983419, -124.6807709998041531 ) ) ;
#6237 = PLANE ( 'NONE',  #5761 ) ;
#6238 = DIRECTION ( 'NONE',  ( 1.000000000000000000, -1.262554838833776231E-16, 0.000000000000000000 ) ) ;
#6239 = FACE_OUTER_BOUND ( 'NONE', #2550, .T. ) ;
#6240 = EDGE_CURVE ( 'NONE', #9573, #10609, #4835, .T. ) ;
#6241 = DIRECTION ( 'NONE',  ( 0.000000000000000000, 1.000000000000000000, 0.000000000000000000 ) ) ;
#6242 = ORIENTED_EDGE ( 'NONE', *, *, #11755, .F. ) ;
#6243 = CARTESIAN_POINT ( 'NONE',  ( 20.72176904448479462, 180.0185442467888493, -123.3140496758510949 ) ) ;
#6244 = AXIS2_PLACEMENT_3D ( 'NONE', #2184, #8734, #5882 ) ;
#6245 = CARTESIAN_POINT ( 'NONE',  ( -379.4184094136624594, 62.42756673384518962, -128.8379558659856059 ) ) ;
#6246 = CARTESIAN_POINT ( 'NONE',  ( -1038.158164256572263, 71.32123499372137587, -154.2940595301283224 ) ) ;
#6247 = CARTESIAN_POINT ( 'NONE',  ( -821.7324155770304515, 74.13196894618619126, -143.0682369473090603 ) ) ;
#6248 = DIRECTION ( 'NONE',  ( 0.000000000000000000, 0.000000000000000000, 1.000000000000000000 ) ) ;
#6249 = DIRECTION ( 'NONE',  ( -0.000000000000000000, -1.000000000000000000, -0.000000000000000000 ) ) ;
#6250 = CYLINDRICAL_SURFACE ( 'NONE', #6216, 7.500000000000007105 ) ;
#6251 = CARTESIAN_POINT ( 'NONE',  ( -828.1700845326885201, 76.17242124353187194, -94.68660788644223203 ) ) ;
#6252 = PRESENTATION_STYLE_ASSIGNMENT (( #11872 ) ) ;
#6253 = FACE_OUTER_BOUND ( 'NONE', #9960, .T. ) ;
#6254 = ORIENTED_EDGE ( 'NONE', *, *, #4260, .T. ) ;
#6255 = CARTESIAN_POINT ( 'NONE',  ( -853.7969483066773364, 45.36294356226267865, -149.7857175106635168 ) ) ;
#6256 = CIRCLE ( 'NONE', #3684, 7.500000000000007105 ) ;
#6257 = ADVANCED_FACE ( 'NONE', ( #7738 ), #8767, .F. ) ;
#6258 = VERTEX_POINT ( 'NONE', #3040 ) ;
#6259 = CARTESIAN_POINT ( 'NONE',  ( -19.97808759892263453, 180.7042479906455696, -126.0868659437894053 ) ) ;
#6260 = ORIENTED_EDGE ( 'NONE', *, *, #5497, .F. ) ;
#6261 = CIRCLE ( 'NONE', #9010, 1.000000000000000888 ) ;
#6262 = CARTESIAN_POINT ( 'NONE',  ( -380.4284056416585713, 64.22849513334448091, -133.8612360355819817 ) ) ;
#6263 = FACE_OUTER_BOUND ( 'NONE', #1898, .T. ) ;
#6264 = EDGE_LOOP ( 'NONE', ( #8562, #8807 ) ) ;
#6265 = EDGE_LOOP ( 'NONE', ( #7537, #10890 ) ) ;
#6266 = CARTESIAN_POINT ( 'NONE',  ( -957.2086549536783195, 47.65337959301152893, -126.6442663926291345 ) ) ;
#6267 = CARTESIAN_POINT ( 'NONE',  ( -828.8285638327242850, 78.67432280806536937, -90.68077099980378364 ) ) ;
#6268 = AXIS2_PLACEMENT_3D ( 'NONE', #3785, #2804, #1883 ) ;
#6269 = CARTESIAN_POINT ( 'NONE',  ( -819.0864923327435463, 80.29251723649532835, -154.5226158375324985 ) ) ;
#6270 = CARTESIAN_POINT ( 'NONE',  ( -1031.956718292106189, 74.21439239895558160, -95.06748246948035330 ) ) ;
#6271 = CARTESIAN_POINT ( 'NONE',  ( 4.808665244885994618E-14, -492.9999999999998863, 141.4213562373094817 ) ) ;
#6272 = CARTESIAN_POINT ( 'NONE',  ( 35.00000000000000000, 152.0000000000000000, -159.6807709998038547 ) ) ;
#6273 = DIRECTION ( 'NONE',  ( 1.186840563529527301E-16, -1.000000000000000000, 0.000000000000000000 ) ) ;
#6274 = ORIENTED_EDGE ( 'NONE', *, *, #10993, .F. ) ;
#6275 = AXIS2_PLACEMENT_3D ( 'NONE', #4509, #10991, #5236 ) ;
#6276 = CARTESIAN_POINT ( 'NONE',  ( -20.84071877255746230, 179.0301507356313664, -123.8425399495678221 ) ) ;
#6277 = CARTESIAN_POINT ( 'NONE',  ( -305.0000000000000568, 12.00000000000001066, -159.6807709998038547 ) ) ;
#6278 = VERTEX_POINT ( 'NONE', #2058 ) ;
#6279 = CARTESIAN_POINT ( 'NONE',  ( -827.5986411883342271, 81.97471746463595821, -154.3043682292991718 ) ) ;
#6280 = CARTESIAN_POINT ( 'NONE',  ( -1038.028607166439997, 78.75533988487829617, -94.48732055948607922 ) ) ;
#6281 = CARTESIAN_POINT ( 'NONE',  ( 6.899999999999999467, -5.196152422706638241, -9.000000000000001776 ) ) ;
#6282 = CARTESIAN_POINT ( 'NONE',  ( -20.96868743328214890, 181.6918789721509881, -124.6171519127913712 ) ) ;
#6283 = AXIS2_PLACEMENT_3D ( 'NONE', #11239, #6528, #10298 ) ;
#6284 = EDGE_CURVE ( 'NONE', #1735, #6424, #2258, .T. ) ;
#6285 = CARTESIAN_POINT ( 'NONE',  ( -824.5038201930738069, 73.70910806073447930, -106.4800466717824037 ) ) ;
#6286 = CARTESIAN_POINT ( 'NONE',  ( -823.9892610140070701, 73.67413949648553739, -142.8653811665924991 ) ) ;
#6287 = LINE ( 'NONE', #10055, #2243 ) ;
#6288 = CARTESIAN_POINT ( 'NONE',  ( 87.04832655144112152, 0.000000000000000000, -217.9289243767383368 ) ) ;
#6289 = CIRCLE ( 'NONE', #156, 19.00000000000000000 ) ;
#6290 = VERTEX_POINT ( 'NONE', #1199 ) ;
#6291 = CARTESIAN_POINT ( 'NONE',  ( 6.899999999999999467, 10.39230484541326938, 0.000000000000000000 ) ) ;
#6292 = CARTESIAN_POINT ( 'NONE',  ( -1021.743962174751232, 119.2557508373789403, -122.7172756069789585 ) ) ;
#6293 = DIRECTION ( 'NONE',  ( -1.000000000000000000, 1.262554838833776231E-16, 0.000000000000000000 ) ) ;
#6294 = DIRECTION ( 'NONE',  ( 0.000000000000000000, 0.000000000000000000, -1.000000000000000000 ) ) ;
#6295 = CARTESIAN_POINT ( 'NONE',  ( 19.97422267005762109, 181.0592659261928077, -123.4551364493730574 ) ) ;
#6296 = AXIS2_PLACEMENT_3D ( 'NONE', #5226, #3251, #8997 ) ;
#6297 = ORIENTED_EDGE ( 'NONE', *, *, #11394, .F. ) ;
#6298 = EDGE_CURVE ( 'NONE', #6278, #154, #1453, .T. ) ;
#6299 = CARTESIAN_POINT ( 'NONE',  ( -120.8820948793972434, 12.00000000000000000, -186.6989091883324363 ) ) ;
#6300 = ADVANCED_FACE ( 'NONE', ( #2294 ), #7174, .T. ) ;
#6301 = DIRECTION ( 'NONE',  ( -8.163404592832030268E-17, 1.000000000000000000, -0.000000000000000000 ) ) ;
#6302 = CARTESIAN_POINT ( 'NONE',  ( -821.5848584200534788, 74.20299736547815428, -143.0985335409777690 ) ) ;
#6303 = ADVANCED_FACE ( 'NONE', ( #4210 ), #4335, .F. ) ;
#6304 =( NAMED_UNIT ( * ) SI_UNIT ( $, .STERADIAN. ) SOLID_ANGLE_UNIT ( ) );
#6305 = DIRECTION ( 'NONE',  ( 0.000000000000000000, -1.000000000000000000, 0.000000000000000000 ) ) ;
#6306 = CARTESIAN_POINT ( 'NONE',  ( -974.9912860506709649, 88.33816101283774458, -154.2940595301278108 ) ) ;
#6307 = CARTESIAN_POINT ( 'NONE',  ( 0.000000000000000000, -6.000000000000000000, -118.9213562373094817 ) ) ;
#6308 = ORIENTED_EDGE ( 'NONE', *, *, #5783, .F. ) ;
#6309 = DIRECTION ( 'NONE',  ( 0.000000000000000000, -1.000000000000000000, 0.000000000000000000 ) ) ;
#6310 = CIRCLE ( 'NONE', #9477, 7.500000000000007105 ) ;
#6311 = ORIENTED_EDGE ( 'NONE', *, *, #11290, .F. ) ;
#6312 = CYLINDRICAL_SURFACE ( 'NONE', #8635, 175.0000000000000284 ) ;
#6313 = CARTESIAN_POINT ( 'NONE',  ( -817.7441816825903516, 35.12288937987674586, -141.4553492942758908 ) ) ;
#6314 = CARTESIAN_POINT ( 'NONE',  ( 20.00000000000000000, 182.6968134406613160, -124.6807709998155076 ) ) ;
#6315 = ORIENTED_EDGE ( 'NONE', *, *, #3995, .T. ) ;
#6316 = VERTEX_POINT ( 'NONE', #11698 ) ;
#6317 = CARTESIAN_POINT ( 'NONE',  ( 20.95930455509759938, 178.7332200987271733, -124.5534165879671207 ) ) ;
#6318 = CARTESIAN_POINT ( 'NONE',  ( -19.89655267018000018, 181.8155712312599519, -126.7144533547834016 ) ) ;
#6319 = EDGE_CURVE ( 'NONE', #6938, #7340, #8578, .T. ) ;
#6320 = ORIENTED_EDGE ( 'NONE', *, *, #2370, .T. ) ;
#6321 = EDGE_CURVE ( 'NONE', #5183, #8245, #2056, .T. ) ;
#6322 = CARTESIAN_POINT ( 'NONE',  ( -372.4518007995145013, 62.11038424318570605, -126.9228541902815692 ) ) ;
#6323 = DIRECTION ( 'NONE',  ( 0.000000000000000000, 0.000000000000000000, 1.000000000000000000 ) ) ;
#6324 = ORIENTED_EDGE ( 'NONE', *, *, #10471, .F. ) ;
#6325 = ORIENTED_EDGE ( 'NONE', *, *, #11233, .T. ) ;
#6326 = DIRECTION ( 'NONE',  ( 0.000000000000000000, 5.522905491341382306E-16, 1.000000000000000000 ) ) ;
#6327 = DIRECTION ( 'NONE',  ( -0.000000000000000000, 0.000000000000000000, -1.000000000000000000 ) ) ;
#6328 = CARTESIAN_POINT ( 'NONE',  ( -1031.632959140997855, 88.47632675500361188, -95.06748246948018277 ) ) ;
#6329 = CARTESIAN_POINT ( 'NONE',  ( -19.03136272649511085, 180.2041921146316668, -134.6807709998038547 ) ) ;
#6330 = CIRCLE ( 'NONE', #828, 7.500000000000007105 ) ;
#6331 = CARTESIAN_POINT ( 'NONE',  ( -20.99127284323103382, 178.6746436565158547, -124.7707208788391284 ) ) ;
#6332 = CARTESIAN_POINT ( 'NONE',  ( 0.000000000000000000, 0.000000000000000000, 0.000000000000000000 ) ) ;
#6333 = CARTESIAN_POINT ( 'NONE',  ( 126.4213562373094959, 0.000000000000000000, -7.500000000000019540 ) ) ;
#6334 = EDGE_LOOP ( 'NONE', ( #2248, #6155 ) ) ;
#6335 = DIRECTION ( 'NONE',  ( 0.000000000000000000, 1.000000000000000000, -0.000000000000000000 ) ) ;
#6336 = CARTESIAN_POINT ( 'NONE',  ( -1020.430183747026263, 74.13649791779302234, -96.78565065507955012 ) ) ;
#6337 = DIRECTION ( 'NONE',  ( 1.000000000000000000, 1.486905836551548832E-16, -0.000000000000000000 ) ) ;
#6338 = DIRECTION ( 'NONE',  ( 0.000000000000000000, 0.000000000000000000, 1.000000000000000000 ) ) ;
#6339 = AXIS2_PLACEMENT_3D ( 'NONE', #6394, #12157, #3600 ) ;
#6340 = CARTESIAN_POINT ( 'NONE',  ( -827.6116171724344213, 75.38904402456984144, -105.8033998852342421 ) ) ;
#6341 = CARTESIAN_POINT ( 'NONE',  ( -19.99337316366387185, 178.8785467397834452, -123.9609963871272100 ) ) ;
#6342 = CARTESIAN_POINT ( 'NONE',  ( -823.4903519156962375, 73.67469885889892112, -142.8656372648659953 ) ) ;
#6343 = CIRCLE ( 'NONE', #9510, 35.00000000000000000 ) ;
#6344 = ORIENTED_EDGE ( 'NONE', *, *, #2675, .F. ) ;
#6345 = CARTESIAN_POINT ( 'NONE',  ( -370.0925635847275998, 56.25177319444339474, -118.8156198848447787 ) ) ;
#6346 = CYLINDRICAL_SURFACE ( 'NONE', #11747, 7.500000000000013323 ) ;
#6347 = VERTEX_POINT ( 'NONE', #11760 ) ;
#6348 = CARTESIAN_POINT ( 'NONE',  ( -187.5000000000000000, 12.00000000000001421, -126.4213562373082453 ) ) ;
#6349 = CARTESIAN_POINT ( 'NONE',  ( -1065.000000000008868, 109.8950841424299512, -113.1262384684097526 ) ) ;
#6350 = EDGE_CURVE ( 'NONE', #368, #1414, #11333, .T. ) ;
#6351 = DIRECTION ( 'NONE',  ( 0.000000000000000000, 0.000000000000000000, 1.000000000000000000 ) ) ;
#6352 = CARTESIAN_POINT ( 'NONE',  ( -247.5000000000000000, -9.213203435596478030, -126.4213562373078190 ) ) ;
#6353 = CARTESIAN_POINT ( 'NONE',  ( 8.099999999999999645, 0.000000000000000000, -6.599999999999998757 ) ) ;
#6354 = VECTOR ( 'NONE', #1593, 999.9999999999998863 ) ;
#6355 = CARTESIAN_POINT ( 'NONE',  ( 19.90865200055529272, 181.4799304009622176, -122.7714319726044607 ) ) ;
#6356 = ORIENTED_EDGE ( 'NONE', *, *, #9016, .F. ) ;
#6357 = ORIENTED_EDGE ( 'NONE', *, *, #9540, .F. ) ;
#6358 = CARTESIAN_POINT ( 'NONE',  ( -45.00000000000000711, 138.9999999999999716, -126.4213562373094959 ) ) ;
#6359 = CARTESIAN_POINT ( 'NONE',  ( 21.06505887627893259, 179.6757939811194547, -126.3352607955414442 ) ) ;
#6360 = CARTESIAN_POINT ( 'NONE',  ( -1019.365209469141632, 93.24061105504456748, -154.2940595301284361 ) ) ;
#6361 = CARTESIAN_POINT ( 'NONE',  ( -372.4316250286643140, 101.9596924382562122, -126.1642065034420028 ) ) ;
#6362 = AXIS2_PLACEMENT_3D ( 'NONE', #3749, #3806, #7401 ) ;
#6363 = CARTESIAN_POINT ( 'NONE',  ( -1.234974037096769894E-14, -8.236864015571812914, 3.733333029993799901 ) ) ;
#6364 = FACE_OUTER_BOUND ( 'NONE', #3131, .T. ) ;
#6365 = DIRECTION ( 'NONE',  ( 0.000000000000000000, -1.156482317317870246E-16, 1.000000000000000000 ) ) ;
#6366 = VERTEX_POINT ( 'NONE', #6934 ) ;
#6367 = CARTESIAN_POINT ( 'NONE',  ( 87.04832655144112152, 12.00000000000000000, -225.4289243767383368 ) ) ;
#6368 = CARTESIAN_POINT ( 'NONE',  ( 0.000000000000000000, -492.9999999999998863, -118.9213562373094817 ) ) ;
#6369 = EDGE_CURVE ( 'NONE', #2533, #3679, #6064, .T. ) ;
#6370 = VERTEX_POINT ( 'NONE', #9831 ) ;
#6371 = DIRECTION ( 'NONE',  ( -0.000000000000000000, -1.000000000000000000, -0.000000000000000000 ) ) ;
#6372 = CARTESIAN_POINT ( 'NONE',  ( -1015.825132819589953, 80.44428838836770979, -154.2940595301284645 ) ) ;
#6373 = EDGE_CURVE ( 'NONE', #8852, #6960, #4425, .T. ) ;
#6374 = CARTESIAN_POINT ( 'NONE',  ( -20.71964524312745226, 180.3430340654693111, -123.3053720114590703 ) ) ;
#6375 = ORIENTED_EDGE ( 'NONE', *, *, #3121, .F. ) ;
#6376 = EDGE_LOOP ( 'NONE', ( #9486, #4204, #2314, #11824 ) ) ;
#6377 = EDGE_CURVE ( 'NONE', #3075, #3632, #4633, .T. ) ;
#6378 = CARTESIAN_POINT ( 'NONE',  ( -21.06252592306710980, 180.0652310508445169, -126.4237660800916245 ) ) ;
#6379 = CARTESIAN_POINT ( 'NONE',  ( -6.106226635438360972E-13, 12.00000000000000000, -244.6807709998039400 ) ) ;
#6380 = AXIS2_PLACEMENT_3D ( 'NONE', #8336, #7400, #11172 ) ;
#6381 = ORIENTED_EDGE ( 'NONE', *, *, #11897, .T. ) ;
#6382 = CARTESIAN_POINT ( 'NONE',  ( -373.3345058608713316, 65.54065180381869027, -136.1221809958202300 ) ) ;
#6383 = CARTESIAN_POINT ( 'NONE',  ( -35.00000000000000000, 152.0000000000000000, 190.3192290001959748 ) ) ;
#6384 = VERTEX_POINT ( 'NONE', #10943 ) ;
#6385 = ORIENTED_EDGE ( 'NONE', *, *, #5082, .F. ) ;
#6386 = CARTESIAN_POINT ( 'NONE',  ( 7.500000000000012434, 25.00000000000002132, -126.4213562373094959 ) ) ;
#6387 = CIRCLE ( 'NONE', #10538, 7.500000000000013323 ) ;
#6388 = EDGE_CURVE ( 'NONE', #5232, #10372, #7869, .T. ) ;
#6389 = CYLINDRICAL_SURFACE ( 'NONE', #4692, 7.500000000000007105 ) ;
#6390 = CARTESIAN_POINT ( 'NONE',  ( 19.98008256664037674, 179.4972950632025857, -125.9865773177933477 ) ) ;
#6391 = CARTESIAN_POINT ( 'NONE',  ( -818.8285638327253082, 79.00501984256794685, -154.6082502017302147 ) ) ;
#6392 = CARTESIAN_POINT ( 'NONE',  ( -853.5732225365160275, 62.99598188221410311, -95.06748246948041015 ) ) ;
#6393 = DIRECTION ( 'NONE',  ( -1.000000000000000000, 0.000000000000000000, 0.000000000000000000 ) ) ;
#6394 = CARTESIAN_POINT ( 'NONE',  ( 35.00000000000000000, 81.99999999999998579, 190.3192290001959748 ) ) ;
#6395 = EDGE_CURVE ( 'NONE', #9788, #6696, #267, .T. ) ;
#6396 = ORIENTED_EDGE ( 'NONE', *, *, #807, .T. ) ;
#6397 = AXIS2_PLACEMENT_3D ( 'NONE', #7373, #9291, #4777 ) ;
#6398 = CARTESIAN_POINT ( 'NONE',  ( -819.3316697785950282, 80.88429704961208699, -144.6519063719966027 ) ) ;
#6399 = AXIS2_PLACEMENT_3D ( 'NONE', #7046, #3160, #2237 ) ;
#6400 = DIRECTION ( 'NONE',  ( 0.000000000000000000, 0.000000000000000000, 1.000000000000000000 ) ) ;
#6401 = CARTESIAN_POINT ( 'NONE',  ( 1.249585401188644101E-12, 0.000000000000000000, -6.421356237309494119 ) ) ;
#6402 = VERTEX_POINT ( 'NONE', #10700 ) ;
#6403 = CARTESIAN_POINT ( 'NONE',  ( -1027.375436305349467, 71.63039521860197567, -96.78565065507956433 ) ) ;
#6404 = CARTESIAN_POINT ( 'NONE',  ( 0.000000000000000000, 11.99999999999999645, -118.9213562373094817 ) ) ;
#6405 = DIRECTION ( 'NONE',  ( -8.163404592832030268E-17, 1.000000000000000000, -0.000000000000000000 ) ) ;
#6406 = EDGE_CURVE ( 'NONE', #9394, #546, #8175, .T. ) ;
#6407 = AXIS2_PLACEMENT_3D ( 'NONE', #10657, #3172, #4847 ) ;
#6408 = AXIS2_PLACEMENT_3D ( 'NONE', #7825, #210, #11476 ) ;
#6409 = CARTESIAN_POINT ( 'NONE',  ( -823.8285638327206470, 78.67432280806529832, -264.6807709998040536 ) ) ;
#6410 = CARTESIAN_POINT ( 'NONE',  ( -19.99589244767088658, 177.7875230617645173, -124.1710050278687447 ) ) ;
#6411 = CARTESIAN_POINT ( 'NONE',  ( -20.00000000000000000, 182.6968134406616002, -124.6807709998189466 ) ) ;
#6412 = EDGE_LOOP ( 'NONE', ( #9630, #6539, #3370, #6095 ) ) ;
#6413 = EDGE_LOOP ( 'NONE', ( #7687, #4956, #2925, #7862 ) ) ;
#6414 = CARTESIAN_POINT ( 'NONE',  ( -45.53315400109751465, 0.000000000000000000, -237.8419396193594650 ) ) ;
#6415 = VERTEX_POINT ( 'NONE', #2473 ) ;
#6416 = CARTESIAN_POINT ( 'NONE',  ( 57.50000000000000000, 0.000000000000000000, 0.000000000000000000 ) ) ;
#6417 = CARTESIAN_POINT ( 'NONE',  ( -1017.840614713424657, 119.3387310954205986, -118.7903414690676556 ) ) ;
#6418 = VECTOR ( 'NONE', #2612, 1000.000000000000000 ) ;
#6419 = AXIS2_PLACEMENT_3D ( 'NONE', #1595, #9072, #4325 ) ;
#6420 = DIRECTION ( 'NONE',  ( -8.163404592832031500E-17, 1.000000000000000000, 0.000000000000000000 ) ) ;
#6421 = CARTESIAN_POINT ( 'NONE',  ( 0.000000000000000000, 152.0000000000000284, -118.9213562373094817 ) ) ;
#6422 = CARTESIAN_POINT ( 'NONE',  ( -371.4336752585604700, 59.93884798725025576, -108.4060072831181714 ) ) ;
#6423 = CARTESIAN_POINT ( 'NONE',  ( 19.98255584530173934, 181.1190424432050179, -125.8592435051848497 ) ) ;
#6424 = VERTEX_POINT ( 'NONE', #10819 ) ;
#6425 = ORIENTED_EDGE ( 'NONE', *, *, #1761, .T. ) ;
#6426 = PRESENTATION_LAYER_ASSIGNMENT (  '', '', ( #9778 ) ) ;
#6427 = CARTESIAN_POINT ( 'NONE',  ( -6.360897667028196044E-14, -492.9999999999998863, -141.4213562373094817 ) ) ;
#6428 = CARTESIAN_POINT ( 'NONE',  ( 1.387778780781445676E-14, 0.000000000000000000, 126.4213562373094959 ) ) ;
#6429 = CARTESIAN_POINT ( 'NONE',  ( -1046.676250823071769, 92.10743237175765330, -152.5758913445291967 ) ) ;
#6430 = CARTESIAN_POINT ( 'NONE',  ( -29.99999999999998579, -9.213203435596451385, -126.4213562373092685 ) ) ;
#6431 = CARTESIAN_POINT ( 'NONE',  ( 0.000000000000000000, 11.99999999999999645, -126.4213562373094959 ) ) ;
#6432 = DIRECTION ( 'NONE',  ( 0.000000000000000000, 0.4999999999999995004, -0.8660254037844389297 ) ) ;
#6433 = CARTESIAN_POINT ( 'NONE',  ( -1015.209561144950953, 93.46821065761417913, -154.2940595301282656 ) ) ;
#6434 = CARTESIAN_POINT ( 'NONE',  ( -270.0000000000000000, -9.213203435596478030, -126.4213562373076059 ) ) ;
#6435 = VERTEX_POINT ( 'NONE', #6006 ) ;
#6436 = DIRECTION ( 'NONE',  ( 0.000000000000000000, -1.000000000000000000, 0.000000000000000000 ) ) ;
#6437 = CARTESIAN_POINT ( 'NONE',  ( -373.5257043960141914, 96.29568266366972296, -149.8465111201311686 ) ) ;
#6438 = ORIENTED_EDGE ( 'NONE', *, *, #564, .F. ) ;
#6439 = CARTESIAN_POINT ( 'NONE',  ( -953.2897746444480163, 79.65961628290892804, -154.2940595301281519 ) ) ;
#6440 = AXIS2_PLACEMENT_3D ( 'NONE', #7514, #6463, #10237 ) ;
#6441 = ORIENTED_EDGE ( 'NONE', *, *, #4123, .F. ) ;
#6442 = ORIENTED_EDGE ( 'NONE', *, *, #12228, .T. ) ;
#6443 = EDGE_CURVE ( 'NONE', #4605, #5780, #3835, .T. ) ;
#6444 = CARTESIAN_POINT ( 'NONE',  ( -21.06592070232479585, 179.5874863403726636, -126.2949583768656368 ) ) ;
#6445 = DIRECTION ( 'NONE',  ( 0.000000000000000000, 1.000000000000000000, 0.000000000000000000 ) ) ;
#6446 = EDGE_CURVE ( 'NONE', #4859, #5830, #9862, .T. ) ;
#6447 = VERTEX_POINT ( 'NONE', #7111 ) ;
#6448 = CARTESIAN_POINT ( 'NONE',  ( -372.4958542361324589, 63.44167550995515370, -145.9033127508436962 ) ) ;
#6449 = CARTESIAN_POINT ( 'NONE',  ( -35.00000000000000000, 11.99999999999998046, 190.3192290001959748 ) ) ;
#6450 = AXIS2_PLACEMENT_3D ( 'NONE', #11345, #2886, #5718 ) ;
#6451 = EDGE_CURVE ( 'NONE', #6496, #2042, #2410, .T. ) ;
#6452 = DIRECTION ( 'NONE',  ( -0.000000000000000000, -0.000000000000000000, -1.000000000000000000 ) ) ;
#6453 = CARTESIAN_POINT ( 'NONE',  ( 0.5590800469813528295, -5.620102221249794638, 8.265697409064607371 ) ) ;
#6454 = CARTESIAN_POINT ( 'NONE',  ( 21.06800383392973686, 179.2720088164683432, -126.0983754789175890 ) ) ;
#6455 = CARTESIAN_POINT ( 'NONE',  ( -1026.284439350007460, 91.37828661775220951, -95.06748246948018277 ) ) ;
#6456 = DIRECTION ( 'NONE',  ( -8.163404592832030268E-17, 1.000000000000000000, -0.000000000000000000 ) ) ;
#6457 = DIRECTION ( 'NONE',  ( -0.000000000000000000, -1.000000000000000000, -1.757987137413040192E-14 ) ) ;
#6458 = CARTESIAN_POINT ( 'NONE',  ( -1014.132585063772808, 52.13780504951625261, -126.6442663926290777 ) ) ;
#6459 = CARTESIAN_POINT ( 'NONE',  ( -820.9141234758983501, 82.74039896267174754, -144.6672699209830739 ) ) ;
#6460 = EDGE_LOOP ( 'NONE', ( #6234, #1755, #1597, #5873 ) ) ;
#6461 = CARTESIAN_POINT ( 'NONE',  ( -824.4888212380172945, 83.64126188030886055, -144.6134169528912423 ) ) ;
#6462 = EDGE_CURVE ( 'NONE', #2042, #8251, #6187, .T. ) ;
#6463 = DIRECTION ( 'NONE',  ( 0.000000000000000000, 0.000000000000000000, 1.000000000000000000 ) ) ;
#6464 = ORIENTED_EDGE ( 'NONE', *, *, #3033, .F. ) ;
#6465 = CIRCLE ( 'NONE', #10216, 7.500000000000007105 ) ;
#6466 = CARTESIAN_POINT ( 'NONE',  ( 6.247927005943220505E-13, -6.000000000000005329, -66.42135623730949590 ) ) ;
#6467 = CARTESIAN_POINT ( 'NONE',  ( -1048.040919118596321, 50.77060569800394063, -103.3307627799636919 ) ) ;
#6468 = AXIS2_PLACEMENT_3D ( 'NONE', #3124, #6896, #1279 ) ;
#6469 = LINE ( 'NONE', #10110, #6091 ) ;
#6470 = CYLINDRICAL_SURFACE ( 'NONE', #4989, 5.000000000000115463 ) ;
#6471 = CARTESIAN_POINT ( 'NONE',  ( 19.83775307229960916, 179.6904364649550132, -127.2232196724678914 ) ) ;
#6472 = CARTESIAN_POINT ( 'NONE',  ( -35.00000000000000000, 152.0000000000000000, -124.6807709998038689 ) ) ;
#6473 = CARTESIAN_POINT ( 'NONE',  ( -19.95511007801529857, 178.2536383623800873, -123.3363847648170974 ) ) ;
#6474 = CARTESIAN_POINT ( 'NONE',  ( -144.0488662551579182, 12.00000000000000000, -146.9077238332691877 ) ) ;
#6475 = VECTOR ( 'NONE', #2297, 1000.000000000000000 ) ;
#6476 = EDGE_LOOP ( 'NONE', ( #5274, #3412, #10767, #10154 ) ) ;
#6477 = ORIENTED_EDGE ( 'NONE', *, *, #10921, .T. ) ;
#6478 = CARTESIAN_POINT ( 'NONE',  ( -371.1276969240240646, 59.03915725236748813, -139.2323628767284731 ) ) ;
#6479 = EDGE_CURVE ( 'NONE', #9727, #1813, #7055, .T. ) ;
#6480 = VERTEX_POINT ( 'NONE', #4525 ) ;
#6481 = CARTESIAN_POINT ( 'NONE',  ( -1011.051362836439694, 118.1813008219151868, -113.1262384684097952 ) ) ;
#6482 = AXIS2_PLACEMENT_3D ( 'NONE', #1776, #11171, #9117 ) ;
#6483 = CARTESIAN_POINT ( 'NONE',  ( 21.06778670191736325, 181.2627243817148610, -125.9916999785174170 ) ) ;
#6484 = DIRECTION ( 'NONE',  ( -8.163404592832030268E-17, 1.000000000000000000, -0.000000000000000000 ) ) ;
#6485 = AXIS2_PLACEMENT_3D ( 'NONE', #930, #10370, #5612 ) ;
#6486 = CARTESIAN_POINT ( 'NONE',  ( 21.06229719140383594, 181.4525311855803125, -125.7460643626238124 ) ) ;
#6487 = EDGE_LOOP ( 'NONE', ( #3353, #3847, #6879, #7407 ) ) ;
#6488 = ORIENTED_EDGE ( 'NONE', *, *, #321, .F. ) ;
#6489 = FACE_OUTER_BOUND ( 'NONE', #10653, .T. ) ;
#6490 = LINE ( 'NONE', #3565, #2864 ) ;
#6491 = CARTESIAN_POINT ( 'NONE',  ( -1018.692594135740137, 105.1726068785159214, -149.7857175106633747 ) ) ;
#6492 = AXIS2_PLACEMENT_3D ( 'NONE', #3134, #6850, #7962 ) ;
#6493 = FACE_BOUND ( 'NONE', #11863, .T. ) ;
#6494 = CARTESIAN_POINT ( 'NONE',  ( -1019.365209469141632, 93.24061105504456748, -154.2940595301284361 ) ) ;
#6495 = CARTESIAN_POINT ( 'NONE',  ( 7.500000000000000000, -10.39230484541326405, 0.000000000000000000 ) ) ;
#6496 = VERTEX_POINT ( 'NONE', #5431 ) ;
#6497 = LINE ( 'NONE', #750, #2157 ) ;
#6498 = CARTESIAN_POINT ( 'NONE',  ( -371.8248261169420630, 102.8498242185334846, -142.9335005713146529 ) ) ;
#6499 = ORIENTED_EDGE ( 'NONE', *, *, #6031, .F. ) ;
#6500 = CARTESIAN_POINT ( 'NONE',  ( -1026.651933061287082, 84.71212313386841686, -154.8742214401230228 ) ) ;
#6501 = AXIS2_PLACEMENT_3D ( 'NONE', #1860, #2848, #6790 ) ;
#6502 = ORIENTED_EDGE ( 'NONE', *, *, #6546, .F. ) ;
#6503 = ORIENTED_EDGE ( 'NONE', *, *, #988, .F. ) ;
#6504 = CARTESIAN_POINT ( 'NONE',  ( -19.98805534415840057, 182.6507228061688579, -125.3893087125330368 ) ) ;
#6505 = DIRECTION ( 'NONE',  ( 0.000000000000000000, 0.000000000000000000, 1.000000000000000000 ) ) ;
#6506 = DIRECTION ( 'NONE',  ( -1.000000000000000000, -0.000000000000000000, 0.000000000000000000 ) ) ;
#6507 = CARTESIAN_POINT ( 'NONE',  ( -1062.810894920117335, 52.92335929224806534, -141.4553492942755781 ) ) ;
#6508 = ORIENTED_EDGE ( 'NONE', *, *, #5465, .F. ) ;
#6509 = CARTESIAN_POINT ( 'NONE',  ( -379.3580220151804383, 62.32607694421552935, -128.2928256996931111 ) ) ;
#6510 = VECTOR ( 'NONE', #8884, 1000.000000000000000 ) ;
#6511 = DIRECTION ( 'NONE',  ( 1.224646799147353207E-16, 1.453460497224676649E-32, 1.000000000000000000 ) ) ;
#6512 = VECTOR ( 'NONE', #9382, 999.9999999999998863 ) ;
#6513 = CARTESIAN_POINT ( 'NONE',  ( -6.360897667028196044E-14, -494.9999999999998863, -141.4213562373094817 ) ) ;
#6514 = CARTESIAN_POINT ( 'NONE',  ( -119.9999999999999858, -9.213203435596451385, -126.4213562373086575 ) ) ;
#6515 = ORIENTED_EDGE ( 'NONE', *, *, #3330, .F. ) ;
#6516 = EDGE_CURVE ( 'NONE', #12134, #7292, #2438, .T. ) ;
#6517 = FACE_OUTER_BOUND ( 'NONE', #7657, .T. ) ;
#6518 = CARTESIAN_POINT ( 'NONE',  ( 151.3258811035896656, 12.00000000000000000, -56.13263083939798292 ) ) ;
#6519 = CARTESIAN_POINT ( 'NONE',  ( 19.98895541933857345, 178.9615149398844665, -125.5256490668303400 ) ) ;
#6520 = CARTESIAN_POINT ( 'NONE',  ( -1065.000000000009095, 65.22545431197600863, -99.57582448894517313 ) ) ;
#6521 = DIRECTION ( 'NONE',  ( 1.000000000000000000, 0.000000000000000000, 0.000000000000000000 ) ) ;
#6522 = ORIENTED_EDGE ( 'NONE', *, *, #6087, .T. ) ;
#6523 = CARTESIAN_POINT ( 'NONE',  ( -821.3235167497176690, 83.01396457509397919, -144.6558853884949087 ) ) ;
#6524 = SHAPE_REPRESENTATION_RELATIONSHIP ( 'NONE' , 'NONE' ,  #1102, #4718 ) ;
#6525 =( NAMED_UNIT ( * ) PLANE_ANGLE_UNIT ( ) SI_UNIT ( $, .RADIAN. ) );
#6526 = EDGE_LOOP ( 'NONE', ( #5558, #11875 ) ) ;
#6527 = CARTESIAN_POINT ( 'NONE',  ( -1028.007066121602975, 60.50166182213163069, -103.3307627799636350 ) ) ;
#6528 = DIRECTION ( 'NONE',  ( -1.000000000000000000, 1.262554838833776231E-16, 0.000000000000000000 ) ) ;
#6529 = CARTESIAN_POINT ( 'NONE',  ( -126.4213562373094959, 12.00000000000000000, -7.499999999999991118 ) ) ;
#6530 = EDGE_CURVE ( 'NONE', #1499, #9384, #8164, .T. ) ;
#6531 = APPLICATION_CONTEXT ( 'automotive_design' ) ;
#6532 = DIRECTION ( 'NONE',  ( -0.000000000000000000, 1.000000000000000000, -0.000000000000000000 ) ) ;
#6533 = CARTESIAN_POINT ( 'NONE',  ( -157.5000000000000000, 139.9999999999999716, -126.4213562373084301 ) ) ;
#6534 = CARTESIAN_POINT ( 'NONE',  ( -20.00030656787924599, 178.6896783452461932, -124.7284307341268459 ) ) ;
#6535 = CARTESIAN_POINT ( 'NONE',  ( -822.4997677527400128, 73.84243176666221586, -142.9416447491877307 ) ) ;
#6536 = VERTEX_POINT ( 'NONE', #8427 ) ;
#6537 = PRODUCT_DEFINITION_SHAPE ( 'NONE', 'NONE',  #12252 ) ;
#6538 = CARTESIAN_POINT ( 'NONE',  ( -374.1531042745066316, 71.13268086833227244, -151.9963463910141286 ) ) ;
#6539 = ORIENTED_EDGE ( 'NONE', *, *, #9097, .T. ) ;
#6540 = CARTESIAN_POINT ( 'NONE',  ( -1022.396981161626059, 109.5926079579672319, -103.3307627799638482 ) ) ;
#6541 = DIRECTION ( 'NONE',  ( -1.000000000000000000, -0.000000000000000000, -0.000000000000000000 ) ) ;
#6542 = EDGE_CURVE ( 'NONE', #1835, #11782, #4034, .T. ) ;
#6543 = CARTESIAN_POINT ( 'NONE',  ( 19.94162086851303428, 182.2847572333868129, -126.2138291093985742 ) ) ;
#6544 = CIRCLE ( 'NONE', #7535, 70.00000000000002842 ) ;
#6545 = ORIENTED_EDGE ( 'NONE', *, *, #9288, .F. ) ;
#6546 = EDGE_CURVE ( 'NONE', #1414, #368, #885, .T. ) ;
#6547 = ORIENTED_EDGE ( 'NONE', *, *, #2747, .T. ) ;
#6548 = DIRECTION ( 'NONE',  ( -0.000000000000000000, 1.000000000000000000, 7.930164461608263644E-17 ) ) ;
#6549 = CARTESIAN_POINT ( 'NONE',  ( 4.335549520754014653E-15, 167.0000000000000000, -124.6807709998038405 ) ) ;
#6550 = CARTESIAN_POINT ( 'NONE',  ( -821.0802431487052218, 81.36881375820613016, -154.2940595301280382 ) ) ;
#6551 = CARTESIAN_POINT ( 'NONE',  ( -372.5499461424406604, 101.5496394262485182, -120.1812972028120470 ) ) ;
#6552 = ADVANCED_FACE ( 'NONE', ( #1743 ), #11932, .F. ) ;
#6553 = EDGE_CURVE ( 'NONE', #11084, #8014, #2853, .T. ) ;
#6554 = FACE_OUTER_BOUND ( 'NONE', #8057, .T. ) ;
#6555 = CARTESIAN_POINT ( 'NONE',  ( 0.000000000000000000, 11.99999999999999645, -126.4213562373094959 ) ) ;
#6556 = DIRECTION ( 'NONE',  ( 0.000000000000000000, 1.000000000000000000, -0.000000000000000000 ) ) ;
#6557 = ORIENTED_EDGE ( 'NONE', *, *, #5365, .F. ) ;
#6558 = LINE ( 'NONE', #2727, #2667 ) ;
#6559 = DIRECTION ( 'NONE',  ( 0.000000000000000000, -0.000000000000000000, 1.000000000000000000 ) ) ;
#6560 = CIRCLE ( 'NONE', #9109, 7.500000000000007105 ) ;
#6561 = CARTESIAN_POINT ( 'NONE',  ( -371.9902837035793368, 102.3136832969389189, -143.7067233690550552 ) ) ;
#6562 = ORIENTED_EDGE ( 'NONE', *, *, #2680, .F. ) ;
#6563 = CARTESIAN_POINT ( 'NONE',  ( -903.0443340174343803, 90.92133391050434454, -154.8742214401225112 ) ) ;
#6564 = ORIENTED_EDGE ( 'NONE', *, *, #468, .F. ) ;
#6565 = EDGE_CURVE ( 'NONE', #8540, #5323, #1670, .T. ) ;
#6566 = ORIENTED_EDGE ( 'NONE', *, *, #8266, .T. ) ;
#6567 = AXIS2_PLACEMENT_3D ( 'NONE', #3934, #7763, #269 ) ;
#6568 = CARTESIAN_POINT ( 'NONE',  ( -19.99960403408873688, 181.6742724572797272, -124.3206507117249799 ) ) ;
#6569 = DIRECTION ( 'NONE',  ( 1.224646799147376133E-16, 1.000000000000000000, 4.955873740258437191E-31 ) ) ;
#6570 = FACE_BOUND ( 'NONE', #283, .T. ) ;
#6571 = CARTESIAN_POINT ( 'NONE',  ( -1028.259718048100012, 56.21337363619606720, -141.4553492942759476 ) ) ;
#6572 = ORIENTED_EDGE ( 'NONE', *, *, #1480, .F. ) ;
#6573 = CARTESIAN_POINT ( 'NONE',  ( -374.9207090424860667, 77.70118234822507475, -144.2684479270019153 ) ) ;
#6574 = CARTESIAN_POINT ( 'NONE',  ( -827.8285638327247398, 78.67432280806536937, -158.6807709998041673 ) ) ;
#6575 = CARTESIAN_POINT ( 'NONE',  ( -383.9497063041636125, 73.38109969229333274, -106.6302449113261872 ) ) ;
#6576 = CARTESIAN_POINT ( 'NONE',  ( -119.9999999999999858, -9.213203435596451385, -126.4213562373086575 ) ) ;
#6577 = LINE ( 'NONE', #8385, #3881 ) ;
#6578 = ORIENTED_EDGE ( 'NONE', *, *, #2590, .T. ) ;
#6579 = DIRECTION ( 'NONE',  ( -0.000000000000000000, 0.000000000000000000, -1.000000000000000000 ) ) ;
#6580 = DIRECTION ( 'NONE',  ( 1.000000000000000000, 0.000000000000000000, 0.000000000000000000 ) ) ;
#6581 = AXIS2_PLACEMENT_3D ( 'NONE', #6653, #10423, #1963 ) ;
#6582 = CARTESIAN_POINT ( 'NONE',  ( -1025.323167507843664, 62.35287014669171413, -103.3307627799636350 ) ) ;
#6583 = CARTESIAN_POINT ( 'NONE',  ( -820.0579670039606981, 81.97422455664163010, -104.6794498541746208 ) ) ;
#6584 = EDGE_LOOP ( 'NONE', ( #4083, #8565, #1931, #2423 ) ) ;
#6585 = FACE_BOUND ( 'NONE', #1750, .T. ) ;
#6586 = DIRECTION ( 'NONE',  ( 0.000000000000000000, 0.000000000000000000, 1.000000000000000000 ) ) ;
#6587 = CARTESIAN_POINT ( 'NONE',  ( -373.3641256762145417, 97.05128668816033155, -100.0945821807713543 ) ) ;
#6588 = ORIENTED_EDGE ( 'NONE', *, *, #7538, .F. ) ;
#6589 = CARTESIAN_POINT ( 'NONE',  ( -1016.863910020555409, 59.13213530333446499, -107.9061927053325576 ) ) ;
#6590 = AXIS2_PLACEMENT_3D ( 'NONE', #10560, #2962, #9513 ) ;
#6591 = CARTESIAN_POINT ( 'NONE',  ( 57.50000000000000000, 0.000000000000000000, 0.000000000000000000 ) ) ;
#6592 = CARTESIAN_POINT ( 'NONE',  ( 0.000000000000000000, -6.000000000000000000, -126.4213562373094959 ) ) ;
#6593 = CARTESIAN_POINT ( 'NONE',  ( -818.8285638327206470, 78.67432280806531253, -104.9592124606049879 ) ) ;
#6594 = DIRECTION ( 'NONE',  ( 0.000000000000000000, -0.5205506085008965167, -0.8538308169592768726 ) ) ;
#6595 = CIRCLE ( 'NONE', #6205, 7.500000000000007105 ) ;
#6596 = ADVANCED_FACE ( 'NONE', ( #10073 ), #8302, .T. ) ;
#6597 = AXIS2_PLACEMENT_3D ( 'NONE', #3272, #11642, #1253 ) ;
#6598 = ORIENTED_EDGE ( 'NONE', *, *, #8266, .F. ) ;
#6599 = DIRECTION ( 'NONE',  ( 0.000000000000000000, 0.000000000000000000, 1.000000000000000000 ) ) ;
#6600 = EDGE_CURVE ( 'NONE', #8092, #4400, #11260, .T. ) ;
#6601 = CARTESIAN_POINT ( 'NONE',  ( -852.8684863605087685, 118.0406360202081970, -136.2353035311977862 ) ) ;
#6602 = ORIENTED_EDGE ( 'NONE', *, *, #8797, .T. ) ;
#6603 = CARTESIAN_POINT ( 'NONE',  ( -974.2138504089111848, 120.9496320545084984, -113.1262384684093547 ) ) ;
#6604 = CARTESIAN_POINT ( 'NONE',  ( 19.99606641939810459, 177.7086604316901060, -125.1339395084417276 ) ) ;
#6605 = AXIS2_PLACEMENT_3D ( 'NONE', #12189, #10131, #1796 ) ;
#6606 = EDGE_CURVE ( 'NONE', #7819, #11268, #682, .T. ) ;
#6607 = CIRCLE ( 'NONE', #4642, 7.500000000000007105 ) ;
#6608 = AXIS2_PLACEMENT_3D ( 'NONE', #9302, #845, #4616 ) ;
#6609 = CARTESIAN_POINT ( 'NONE',  ( -1045.864486809339951, 115.5688325305733741, -122.7172756069790438 ) ) ;
#6610 = VERTEX_POINT ( 'NONE', #12127 ) ;
#6611 = CARTESIAN_POINT ( 'NONE',  ( -904.2101318205999405, 125.2895275102983419, -124.6807709998041531 ) ) ;
#6612 = CARTESIAN_POINT ( 'NONE',  ( 1.561981751485805177E-12, -6.000000000000006217, 31.07864376269051121 ) ) ;
#6613 = DIRECTION ( 'NONE',  ( 0.000000000000000000, 1.000000000000000000, 0.000000000000000000 ) ) ;
#6614 = CARTESIAN_POINT ( 'NONE',  ( -1031.197907781699314, 107.2697845108579173, -146.0307792196445291 ) ) ;
#6615 = CIRCLE ( 'NONE', #4650, 7.500000000000013323 ) ;
#6616 = LINE ( 'NONE', #7785, #1093 ) ;
#6617 = AXIS2_PLACEMENT_3D ( 'NONE', #6434, #10017, #5368 ) ;
#6618 = EDGE_LOOP ( 'NONE', ( #4528, #3458, #676, #938 ) ) ;
#6619 = EDGE_CURVE ( 'NONE', #647, #8782, #11002, .T. ) ;
#6620 = CARTESIAN_POINT ( 'NONE',  ( -370.9145534060840532, 105.5813659013322479, -138.0025389308291608 ) ) ;
#6621 = EDGE_LOOP ( 'NONE', ( #4076, #8724 ) ) ;
#6622 = CARTESIAN_POINT ( 'NONE',  ( -975.1903095749692056, 79.73237568579439483, -154.8742214401228523 ) ) ;
#6623 = DIRECTION ( 'NONE',  ( -0.000000000000000000, 1.000000000000000000, -0.000000000000000000 ) ) ;
#6624 = ORIENTED_EDGE ( 'NONE', *, *, #2903, .F. ) ;
#6625 = MECHANICAL_DESIGN_GEOMETRIC_PRESENTATION_REPRESENTATION (  '', ( #9778 ), #1111 ) ;
#6626 = LINE ( 'NONE', #5691, #10996 ) ;
#6627 = VERTEX_POINT ( 'NONE', #1547 ) ;
#6628 = DIRECTION ( 'NONE',  ( 0.000000000000000000, 0.000000000000000000, 1.000000000000000000 ) ) ;
#6629 = CARTESIAN_POINT ( 'NONE',  ( -824.9897882054075353, 73.80822682503037413, -106.4353286633425029 ) ) ;
#6630 = CARTESIAN_POINT ( 'NONE',  ( -374.8135003541144101, 87.17728863486301805, -154.1080623301308208 ) ) ;
#6631 = FACE_OUTER_BOUND ( 'NONE', #10439, .T. ) ;
#6632 = CARTESIAN_POINT ( 'NONE',  ( -384.8761410539145231, 79.01556305096559640, -104.9019531990182088 ) ) ;
#6634 = ADVANCED_FACE ( 'NONE', ( #6493, #9210 ), #10269, .F. ) ;
#6633 = DIRECTION ( 'NONE',  ( -8.163404592832030268E-17, 1.000000000000000000, -0.000000000000000000 ) ) ;
#6635 = ORIENTED_EDGE ( 'NONE', *, *, #11042, .T. ) ;
#6636 = DIRECTION ( 'NONE',  ( 0.000000000000000000, 1.000000000000000000, 0.000000000000000000 ) ) ;
#6637 = PRODUCT ( 'Handle', 'Handle', '', ( #3989 ) ) ;
#6638 = DIRECTION ( 'NONE',  ( 2.040851148208007875E-17, -1.000000000000000000, -0.000000000000000000 ) ) ;
#6639 = CYLINDRICAL_SURFACE ( 'NONE', #3403, 7.500000000000007105 ) ;
#6640 = DIRECTION ( 'NONE',  ( -1.000000000000000000, -0.000000000000000000, -0.000000000000000000 ) ) ;
#6641 = CARTESIAN_POINT ( 'NONE',  ( -927.9936929689729368, 74.21188826700399943, -99.57582448894522997 ) ) ;
#6642 = CARTESIAN_POINT ( 'NONE',  ( -144.0488662551579182, 0.000000000000000000, -146.9077238332691877 ) ) ;
#6643 = CIRCLE ( 'NONE', #314, 7.500000000000007105 ) ;
#6644 = ORIENTED_EDGE ( 'NONE', *, *, #1131, .T. ) ;
#6645 = CARTESIAN_POINT ( 'NONE',  ( -828.8285638327206470, 78.99577924834029830, -144.4565372401586956 ) ) ;
#6646 = PRODUCT_CONTEXT ( 'NONE', #5894, 'mechanical' ) ;
#6647 = CARTESIAN_POINT ( 'NONE',  ( -370.4401466759219375, 106.8513018378076964, -134.3428354745942102 ) ) ;
#6648 = VERTEX_POINT ( 'NONE', #3511 ) ;
#6649 = CARTESIAN_POINT ( 'NONE',  ( -232.4999999999999716, -9.213203435596478030, -126.4213562373078190 ) ) ;
#6650 = CARTESIAN_POINT ( 'NONE',  ( -1013.392840968506675, 67.31954129910425877, -99.57582448894551419 ) ) ;
#6651 = CARTESIAN_POINT ( 'NONE',  ( -277.5000000000000000, 151.9999999999999716, -126.4213562373076059 ) ) ;
#6652 = LINE ( 'NONE', #5356, #6804 ) ;
#6653 = CARTESIAN_POINT ( 'NONE',  ( 0.000000000000000000, -492.9999999999998863, -126.4213562373094959 ) ) ;
#6654 = CARTESIAN_POINT ( 'NONE',  ( 19.97747437608540721, 179.8319032282986143, -126.1164657578071058 ) ) ;
#6655 = PRODUCT_DEFINITION_CONTEXT ( 'detailed design', #1016, 'design' ) ;
#6656 = CARTESIAN_POINT ( 'NONE',  ( -974.2138504089111848, 120.9496320545084984, -113.1262384684093547 ) ) ;
#6657 = FACE_BOUND ( 'NONE', #5, .T. ) ;
#6658 = ORIENTED_EDGE ( 'NONE', *, *, #9624, .F. ) ;
#6659 = CARTESIAN_POINT ( 'NONE',  ( -374.9651464077482501, 79.71832840036303480, -154.5744145532411267 ) ) ;
#6660 = CARTESIAN_POINT ( 'NONE',  ( -373.4738573936541570, 97.83297831077017293, -112.3786037173117194 ) ) ;
#6661 = ORIENTED_EDGE ( 'NONE', *, *, #11821, .T. ) ;
#6662 = CARTESIAN_POINT ( 'NONE',  ( -1025.296800000965050, 108.9225844456047696, -103.3307627799635782 ) ) ;
#6663 = CARTESIAN_POINT ( 'NONE',  ( -926.5908784743301112, 123.4113341959662762, -136.2353035311976441 ) ) ;
#6664 = CARTESIAN_POINT ( 'NONE',  ( 1.249585401188644101E-12, 152.0000000000000000, -6.421356237309483461 ) ) ;
#6665 = EDGE_CURVE ( 'NONE', #4471, #2921, #7585, .T. ) ;
#6666 = AXIS2_PLACEMENT_3D ( 'NONE', #134, #9480, #956 ) ;
#6667 = ADVANCED_FACE ( 'NONE', ( #6364 ), #2912, .T. ) ;
#6668 = CARTESIAN_POINT ( 'NONE',  ( -1017.810720698610226, 119.7719591276204625, -122.7172756069789017 ) ) ;
#6669 = VERTEX_POINT ( 'NONE', #5681 ) ;
#6670 = CARTESIAN_POINT ( 'NONE',  ( 3.123963502971610252E-13, -6.000000000000005329, -96.42135623730949590 ) ) ;
#6671 = DIRECTION ( 'NONE',  ( -1.000000000000000000, 0.000000000000000000, 0.000000000000000000 ) ) ;
#6672 = FACE_OUTER_BOUND ( 'NONE', #701, .T. ) ;
#6673 = CARTESIAN_POINT ( 'NONE',  ( -853.0139081111152564, 107.1087209265616735, -146.0307792196445291 ) ) ;
#6674 = B_SPLINE_CURVE_WITH_KNOTS ( 'NONE', 3,
 ( #10979, #457, #3364, #4252, #6282, #8022, #11790, #3308, #7086, #10915, #9926, #2445, #6228, #9992, #2507, #5282 ),
 .UNSPECIFIED., .F., .F.,
 ( 4, 2, 2, 2, 2, 2, 2, 4 ),
 ( 0.004753387881373966409, 0.005750299331856708294, 0.006248755057098098753, 0.006747210782339490079, 0.007245666507580881405, 0.007744122232822271863, 0.008242577958063662322, 0.008741033683305053648 ),
 .UNSPECIFIED. ) ;
#6675 = DIRECTION ( 'NONE',  ( 0.000000000000000000, 0.000000000000000000, 1.000000000000000000 ) ) ;
#6676 = ORIENTED_EDGE ( 'NONE', *, *, #2393, .T. ) ;
#6677 = CARTESIAN_POINT ( 'NONE',  ( -374.5052761646434192, 91.59736101580315903, -142.2979785311488286 ) ) ;
#6678 = DIRECTION ( 'NONE',  ( -0.000000000000000000, -1.000000000000000000, -0.000000000000000000 ) ) ;
#6679 = EDGE_CURVE ( 'NONE', #9394, #1855, #1986, .T. ) ;
#6680 = VERTEX_POINT ( 'NONE', #5743 ) ;
#6681 = VECTOR ( 'NONE', #6337, 1000.000000000000000 ) ;
#6682 = ORIENTED_EDGE ( 'NONE', *, *, #4123, .T. ) ;
#6683 = CARTESIAN_POINT ( 'NONE',  ( 19.97333794400199025, 179.3704271068745868, -123.4361500813402017 ) ) ;
#6684 = CARTESIAN_POINT ( 'NONE',  ( -828.3216978517767757, 80.87401637003937083, -144.6495766896184421 ) ) ;
#6685 = CARTESIAN_POINT ( 'NONE',  ( -821.5852935318529262, 74.19369191907395589, -106.2666214282633490 ) ) ;
#6686 = CARTESIAN_POINT ( 'NONE',  ( -954.0832773815118344, 60.15510303592687080, -146.0307792196447565 ) ) ;
#6687 = VERTEX_POINT ( 'NONE', #3770 ) ;
#6688 = CARTESIAN_POINT ( 'NONE',  ( -374.9845254985059455, 80.12302501620320072, -144.5988415073323665 ) ) ;
#6689 = DIRECTION ( 'NONE',  ( -0.000000000000000000, -1.000000000000000000, -1.757987137413040192E-14 ) ) ;
#6690 = CARTESIAN_POINT ( 'NONE',  ( -384.1592857098779632, 74.28227529662643747, -106.2268997244850652 ) ) ;
#6691 = DIRECTION ( 'NONE',  ( 3.061276722312011504E-17, -1.000000000000000000, -0.000000000000000000 ) ) ;
#6692 = AXIS2_PLACEMENT_3D ( 'NONE', #3950, #3024, #7601 ) ;
#6693 = ORIENTED_EDGE ( 'NONE', *, *, #1319, .T. ) ;
#6694 = CARTESIAN_POINT ( 'NONE',  ( -1017.027421246632343, 56.01181809833700243, -136.2353035311990368 ) ) ;
#6695 = VECTOR ( 'NONE', #8482, 1000.000000000000000 ) ;
#6696 = VERTEX_POINT ( 'NONE', #2849 ) ;
#6697 = ADVANCED_FACE ( 'NONE', ( #4710 ), #4820, .F. ) ;
#6698 = EDGE_CURVE ( 'NONE', #7241, #64, #6988, .T. ) ;
#6699 = CARTESIAN_POINT ( 'NONE',  ( -928.1401715908999677, 69.16346707076998257, -103.3307627799636919 ) ) ;
#6700 = CIRCLE ( 'NONE', #2955, 57.99999999999999289 ) ;
#6701 = CARTESIAN_POINT ( 'NONE',  ( -819.0811117622716893, 80.27710935352847343, -104.7528066153024042 ) ) ;
#6702 = ORIENTED_EDGE ( 'NONE', *, *, #5405, .T. ) ;
#6703 = CARTESIAN_POINT ( 'NONE',  ( -383.7561884827940730, 72.61679055868643218, -107.0088101474849793 ) ) ;
#6704 = LINE ( 'NONE', #9833, #1174 ) ;
#6705 = ORIENTED_EDGE ( 'NONE', *, *, #7262, .T. ) ;
#6706 = DIRECTION ( 'NONE',  ( 1.000000000000000000, 0.000000000000000000, 0.000000000000000000 ) ) ;
#6707 = CARTESIAN_POINT ( 'NONE',  ( -372.2669691774863736, 101.3813217465900323, -104.4136360144974134 ) ) ;
#6708 = ORIENTED_EDGE ( 'NONE', *, *, #4290, .T. ) ;
#6709 = CARTESIAN_POINT ( 'NONE',  ( -902.4158961391592584, 71.79205886009090420, -99.57582448894511629 ) ) ;
#6710 = DIRECTION ( 'NONE',  ( -2.081668171172161734E-17, -4.930380657631307143E-31, 1.000000000000000000 ) ) ;
#6711 = CARTESIAN_POINT ( 'NONE',  ( -187.5000000000000000, 151.9999999999999716, -126.4213562373082453 ) ) ;
#6712 = CARTESIAN_POINT ( 'NONE',  ( 0.000000000000000000, 152.0000000000000000, -124.6807709998038689 ) ) ;
#6713 = CARTESIAN_POINT ( 'NONE',  ( 0.000000000000000000, -494.9999999999998863, -126.4213562373094959 ) ) ;
#6714 = CARTESIAN_POINT ( 'NONE',  ( 35.00000000000000000, 139.9999999999999716, -89.68077099980384048 ) ) ;
#6715 = CARTESIAN_POINT ( 'NONE',  ( -19.98540286720293579, 179.1181071172495081, -125.7109378457173676 ) ) ;
#6716 = DIRECTION ( 'NONE',  ( -1.000000000000000000, -0.000000000000000000, -0.000000000000000000 ) ) ;
#6717 = VERTEX_POINT ( 'NONE', #231 ) ;
#6718 = CARTESIAN_POINT ( 'NONE',  ( -381.2985570915043922, 98.03646409573219955, -112.7250802902767219 ) ) ;
#6719 = VERTEX_POINT ( 'NONE', #7543 ) ;
#6720 = CARTESIAN_POINT ( 'NONE',  ( -822.7482738817717518, 104.4536172844453858, -103.3307627799637203 ) ) ;
#6721 = DIRECTION ( 'NONE',  ( 0.000000000000000000, 0.000000000000000000, -1.000000000000000000 ) ) ;
#6722 = DIRECTION ( 'NONE',  ( -0.000000000000000000, -1.000000000000000000, -0.000000000000000000 ) ) ;
#6723 = CARTESIAN_POINT ( 'NONE',  ( -1030.931480980269043, 117.9615145441170654, -122.7172756069790722 ) ) ;
#6724 = ORIENTED_EDGE ( 'NONE', *, *, #6451, .T. ) ;
#6725 = DIRECTION ( 'NONE',  ( -1.000000000000000000, 0.000000000000000000, 0.000000000000000000 ) ) ;
#6726 = DIRECTION ( 'NONE',  ( -0.000000000000000000, 1.189524669241239115E-16, -1.000000000000000000 ) ) ;
#6727 = CARTESIAN_POINT ( 'NONE',  ( -992.1517139731079169, 115.6613254010897123, -141.4553492942762318 ) ) ;
#6728 = CIRCLE ( 'NONE', #9696, 45.00000000000000711 ) ;
#6729 = DIRECTION ( 'NONE',  ( -0.000000000000000000, 1.000000000000000000, -0.000000000000000000 ) ) ;
#6730 = CARTESIAN_POINT ( 'NONE',  ( 7.500000000000000000, 0.000000000000000000, 0.000000000000000000 ) ) ;
#6731 =( NAMED_UNIT ( * ) PLANE_ANGLE_UNIT ( ) SI_UNIT ( $, .RADIAN. ) );
#6732 = VERTEX_POINT ( 'NONE', #9583 ) ;
#6733 = CARTESIAN_POINT ( 'NONE',  ( 20.00000000000011724, 182.6813753181032496, -124.4861612253857004 ) ) ;
#6734 = PRODUCT ( 'Long Manual Ratchet Lever Handle', 'Long Manual Ratchet Lever Handle', '', ( #6646 ) ) ;
#6735 = CARTESIAN_POINT ( 'NONE',  ( -1060.958858734060186, 107.4804882715809526, -141.4553492942761750 ) ) ;
#6736 = CARTESIAN_POINT ( 'NONE',  ( 35.00000000000000000, 0.000000000000000000, 190.3192290001959464 ) ) ;
#6737 = VERTEX_POINT ( 'NONE', #2107 ) ;
#6738 = EDGE_LOOP ( 'NONE', ( #4756, #8320, #10194, #5505, #832, #852, #1339, #4468, #8355, #10823 ) ) ;
#6739 = LINE ( 'NONE', #5810, #482 ) ;
#6740 = DIRECTION ( 'NONE',  ( -0.000000000000000000, 1.000000000000000000, 7.930164461608263644E-17 ) ) ;
#6741 = CARTESIAN_POINT ( 'NONE',  ( -1065.000000000001364, 65.22545431197576704, -149.7857175106635168 ) ) ;
#6742 = CIRCLE ( 'NONE', #3367, 7.500000000000012434 ) ;
#6743 = EDGE_CURVE ( 'NONE', #8630, #11262, #6616, .T. ) ;
#6744 = CARTESIAN_POINT ( 'NONE',  ( -374.4862286338727699, 72.16765808346663391, -142.2089878380306800 ) ) ;
#6745 = CARTESIAN_POINT ( 'NONE',  ( -59.99999999999998579, 24.00000000000001421, -126.4213562373090696 ) ) ;
#6746 = CARTESIAN_POINT ( 'NONE',  ( -374.7871828591273697, 75.45048456915552038, -105.7389799933290817 ) ) ;
#6747 = EDGE_CURVE ( 'NONE', #8838, #7020, #8777, .T. ) ;
#6748 = DIRECTION ( 'NONE',  ( 1.000000000000000000, -0.000000000000000000, -0.000000000000000000 ) ) ;
#6749 = VECTOR ( 'NONE', #1614, 1000.000000000000000 ) ;
#6750 = VERTEX_POINT ( 'NONE', #8537 ) ;
#6751 = ADVANCED_FACE ( 'NONE', ( #8660 ), #7393, .F. ) ;
#6752 = DIRECTION ( 'NONE',  ( -0.000000000000000000, -1.000000000000000000, -0.000000000000000000 ) ) ;
#6753 = VECTOR ( 'NONE', #4647, 1000.000000000000000 ) ;
#6754 = CARTESIAN_POINT ( 'NONE',  ( -975.9242088207895449, 48.36955882740807766, -103.3307627799632513 ) ) ;
#6755 = CARTESIAN_POINT ( 'NONE',  ( -828.8285638327245124, 78.83536470145031672, -104.9320557148181479 ) ) ;
#6756 = CARTESIAN_POINT ( 'NONE',  ( -928.4218612484578443, 59.99049470396625594, -130.5712005305400965 ) ) ;
#6757 = EDGE_LOOP ( 'NONE', ( #5682, #6522 ) ) ;
#6758 =( REPRESENTATION_RELATIONSHIP ('NONE','NONE', #12149, #12068 ) REPRESENTATION_RELATIONSHIP_WITH_TRANSFORMATION ( #5028 )SHAPE_REPRESENTATION_RELATIONSHIP( ) );
#6759 = CARTESIAN_POINT ( 'NONE',  ( -827.5977362841322247, 75.37243826020210236, -154.6813451849070304 ) ) ;
#6760 = EDGE_LOOP ( 'NONE', ( #3220, #4352 ) ) ;
#6761 = DIRECTION ( 'NONE',  ( -1.000000000000000000, -0.000000000000000000, -0.000000000000000000 ) ) ;
#6762 = APPLICATION_PROTOCOL_DEFINITION ( 'draft international standard', 'automotive_design', 1998, #4004 ) ;
#6763 = ORIENTED_EDGE ( 'NONE', *, *, #2513, .F. ) ;
#6764 = CARTESIAN_POINT ( 'NONE',  ( -1032.589060384100776, 47.36392975189028931, -113.1262384684095537 ) ) ;
#6765 = EDGE_CURVE ( 'NONE', #4471, #7628, #7606, .T. ) ;
#6766 = FACE_OUTER_BOUND ( 'NONE', #9946, .T. ) ;
#6767 = CARTESIAN_POINT ( 'NONE',  ( 35.00000000000000000, 81.99999999999998579, 190.3192290001959748 ) ) ;
#6768 = FACE_BOUND ( 'NONE', #346, .T. ) ;
#6769 = UNCERTAINTY_MEASURE_WITH_UNIT (LENGTH_MEASURE( 1.000000000000000082E-05 ), #4246, 'distance_accuracy_value', 'NONE');
#6770 = EDGE_CURVE ( 'NONE', #7628, #4476, #10353, .T. ) ;
#6771 = CARTESIAN_POINT ( 'NONE',  ( -991.8293279264787543, 119.7328159579555091, -113.1262384684096673 ) ) ;
#6772 = CARTESIAN_POINT ( 'NONE',  ( 19.03136272649511085, 180.2041921146316668, -134.6807709998038547 ) ) ;
#6773 = LINE ( 'NONE', #3999, #1084 ) ;
#6774 = ORIENTED_EDGE ( 'NONE', *, *, #708, .T. ) ;
#6775 = CARTESIAN_POINT ( 'NONE',  ( 1.959217102279688941E-15, 139.9999999999999716, -126.4213562373094959 ) ) ;
#6776 = CARTESIAN_POINT ( 'NONE',  ( -384.5214733245267666, 87.83340981944037651, -105.5475429248750032 ) ) ;
#6777 = FILL_AREA_STYLE ('',( #7957 ) ) ;
#6778 = EDGE_LOOP ( 'NONE', ( #12021, #4214 ) ) ;
#6779 = CARTESIAN_POINT ( 'NONE',  ( -1031.329434936836833, 101.6864263019767378, -99.57582448894520155 ) ) ;
#6780 = EDGE_CURVE ( 'NONE', #7586, #6370, #6012, .T. ) ;
#6781 = CARTESIAN_POINT ( 'NONE',  ( -210.0000000000000000, -9.213203435596478030, -126.4213562373080180 ) ) ;
#6782 = VECTOR ( 'NONE', #3734, 1000.000000000000000 ) ;
#6783 = AXIS2_PLACEMENT_3D ( 'NONE', #8106, #8895, #6990 ) ;
#6784 = CARTESIAN_POINT ( 'NONE',  ( 0.000000000000000000, 152.0000000000000000, -124.6807709998038689 ) ) ;
#6785 = ORIENTED_EDGE ( 'NONE', *, *, #2835, .F. ) ;
#6786 = CARTESIAN_POINT ( 'NONE',  ( 57.50000000000000000, 0.000000000000000000, 5.035999999999999588 ) ) ;
#6787 = CARTESIAN_POINT ( 'NONE',  ( -818.9856806503953521, 79.95950042231982025, -104.7825536331197043 ) ) ;
#6788 = CARTESIAN_POINT ( 'NONE',  ( 120.8820948793965186, 12.00000000000000000, -194.1989091883332890 ) ) ;
#6789 = CARTESIAN_POINT ( 'NONE',  ( -1037.461794897090840, 110.6138330393710731, -141.4553492942763171 ) ) ;
#6790 = DIRECTION ( 'NONE',  ( -1.000000000000000000, 0.000000000000000000, 0.000000000000000000 ) ) ;
#6791 = DIRECTION ( 'NONE',  ( -8.163404592832030268E-17, 1.000000000000000000, -0.000000000000000000 ) ) ;
#6792 = DIRECTION ( 'NONE',  ( -0.000000000000000000, 1.000000000000000000, 7.930164461608263644E-17 ) ) ;
#6793 = EDGE_LOOP ( 'NONE', ( #3710, #1617 ) ) ;
#6794 = AXIS2_PLACEMENT_3D ( 'NONE', #4388, #10013, #1543 ) ;
#6795 = AXIS2_PLACEMENT_3D ( 'NONE', #1123, #7664, #10380 ) ;
#6796 = CIRCLE ( 'NONE', #11748, 7.500000000000007105 ) ;
#6797 = DIRECTION ( 'NONE',  ( 0.000000000000000000, 0.000000000000000000, -1.000000000000000000 ) ) ;
#6798 = CARTESIAN_POINT ( 'NONE',  ( -1018.401127491266152, 110.2021201405462136, -146.0307792196445860 ) ) ;
#6799 = FACE_BOUND ( 'NONE', #11590, .T. ) ;
#6800 = ORIENTED_EDGE ( 'NONE', *, *, #566, .T. ) ;
#6801 = ORIENTED_EDGE ( 'NONE', *, *, #342, .F. ) ;
#6802 = CARTESIAN_POINT ( 'NONE',  ( 19.95730553998325973, 178.2270339500159650, -123.3692462230967521 ) ) ;
#6803 = CARTESIAN_POINT ( 'NONE',  ( -127.4999999999999716, 24.00000000000001421, -126.4213562373086575 ) ) ;
#6804 = VECTOR ( 'NONE', #11920, 1000.000000000000000 ) ;
#6805 = FACE_OUTER_BOUND ( 'NONE', #7494, .T. ) ;
#6806 = DIRECTION ( 'NONE',  ( 1.000000000000000000, 0.000000000000000000, -0.000000000000000000 ) ) ;
#6807 = CARTESIAN_POINT ( 'NONE',  ( -1047.626240907250804, 63.12837257276900260, -152.5758913445295093 ) ) ;
#6808 = DIRECTION ( 'NONE',  ( -1.000000000000000000, 0.000000000000000000, 0.000000000000000000 ) ) ;
#6809 = ORIENTED_EDGE ( 'NONE', *, *, #2319, .T. ) ;
#6810 = CARTESIAN_POINT ( 'NONE',  ( -374.2117181976924485, 71.51684740197940471, -152.1890516768436612 ) ) ;
#6811 = DIRECTION ( 'NONE',  ( 0.000000000000000000, 1.689469820081754479E-14, -1.000000000000000000 ) ) ;
#6812 = CARTESIAN_POINT ( 'NONE',  ( -374.1390116440427960, 69.71711930496753951, -108.8128785988674849 ) ) ;
#6813 = EDGE_LOOP ( 'NONE', ( #10508, #11047, #10675, #8494 ) ) ;
#6814 = CIRCLE ( 'NONE', #1485, 20.00000000000017053 ) ;
#6815 = CIRCLE ( 'NONE', #10960, 7.500000000000007105 ) ;
#6816 = EDGE_LOOP ( 'NONE', ( #7795, #11766 ) ) ;
#6817 = EDGE_CURVE ( 'NONE', #6480, #11140, #11433, .T. ) ;
#6818 = ORIENTED_EDGE ( 'NONE', *, *, #93, .T. ) ;
#6819 = LINE ( 'NONE', #2992, #720 ) ;
#6820 = EDGE_CURVE ( 'NONE', #8735, #8014, #3026, .T. ) ;
#6821 = CARTESIAN_POINT ( 'NONE',  ( -795.0000000000020464, 54.10491585757070965, -113.1262384684093121 ) ) ;
#6822 = FACE_OUTER_BOUND ( 'NONE', #8422, .T. ) ;
#6823 = CARTESIAN_POINT ( 'NONE',  ( -822.0624079427843753, 83.35484814232698625, -104.7266156443422176 ) ) ;
#6824 = CARTESIAN_POINT ( 'NONE',  ( -1032.589060384111690, 47.36392975189053800, -136.2353035311989231 ) ) ;
#6825 = ORIENTED_EDGE ( 'NONE', *, *, #6395, .F. ) ;
#6826 =( GEOMETRIC_REPRESENTATION_CONTEXT ( 3 ) GLOBAL_UNCERTAINTY_ASSIGNED_CONTEXT ( ( #5095 ) ) GLOBAL_UNIT_ASSIGNED_CONTEXT ( ( #5744, #6731, #7487 ) ) REPRESENTATION_CONTEXT ( 'NONE', 'WORKASPACE' ) );
#6827 = CARTESIAN_POINT ( 'NONE',  ( -384.7926048166160058, 85.88261479689718669, -105.0522379990735544 ) ) ;
#6828 = CARTESIAN_POINT ( 'NONE',  ( 3.123963502971610252E-13, 0.000000000000000000, -96.42135623730949590 ) ) ;
#6829 = EDGE_LOOP ( 'NONE', ( #7429, #5435, #4946, #12144, #179, #5657, #6724, #2834, #9003, #3940 ) ) ;
#6830 = VERTEX_POINT ( 'NONE', #4937 ) ;
#6831 = CARTESIAN_POINT ( 'NONE',  ( -1028.611899521406713, 50.57492120214472919, -122.7172756069792428 ) ) ;
#6832 = CARTESIAN_POINT ( 'NONE',  ( -305.0000000000000568, 12.00000000000001066, -89.68077099980384048 ) ) ;
#6833 = CYLINDRICAL_SURFACE ( 'NONE', #12142, 7.500000000000007105 ) ;
#6834 = PRODUCT_DEFINITION_FORMATION_WITH_SPECIFIED_SOURCE ( 'ANY', '', #6734, .NOT_KNOWN. ) ;
#6835 = UNCERTAINTY_MEASURE_WITH_UNIT (LENGTH_MEASURE( 1.000000000000000082E-05 ), #7077, 'distance_accuracy_value', 'NONE');
#6836 = VECTOR ( 'NONE', #11460, 1000.000000000000000 ) ;
#6837 = CARTESIAN_POINT ( 'NONE',  ( -823.1749794181283733, 110.1592441374100844, -107.9061927053325292 ) ) ;
#6838 = CARTESIAN_POINT ( 'NONE',  ( -819.8285638327242850, 78.67432280806536937, -90.68077099980378364 ) ) ;
#6839 = EDGE_CURVE ( 'NONE', #11763, #11346, #1282, .T. ) ;
#6840 = ORIENTED_EDGE ( 'NONE', *, *, #11739, .F. ) ;
#6841 = CARTESIAN_POINT ( 'NONE',  ( 144.0488662551573782, 12.00000000000000000, -146.9077238332702109 ) ) ;
#6842 = CARTESIAN_POINT ( 'NONE',  ( -384.6205072238515186, 87.19846374239256193, -105.3653610531364251 ) ) ;
#6843 = EDGE_CURVE ( 'NONE', #2015, #1622, #11372, .T. ) ;
#6844 = ORIENTED_EDGE ( 'NONE', *, *, #10817, .T. ) ;
#6845 = DIRECTION ( 'NONE',  ( 3.061276722312011504E-17, -1.000000000000000000, 0.000000000000000000 ) ) ;
#6846 = CARTESIAN_POINT ( 'NONE',  ( -903.6727718956999524, 110.0506089609176712, -99.57582448894470417 ) ) ;
#6847 = CIRCLE ( 'NONE', #1508, 7.500000000000007105 ) ;
#6848 = ORIENTED_EDGE ( 'NONE', *, *, #9702, .T. ) ;
#6849 = CARTESIAN_POINT ( 'NONE',  ( -795.0000000000021600, 107.1049510380564129, -141.4553492942762318 ) ) ;
#6850 = DIRECTION ( 'NONE',  ( -0.000000000000000000, -1.000000000000000000, -0.000000000000000000 ) ) ;
#6851 = CARTESIAN_POINT ( 'NONE',  ( -1065.000000000006594, 112.0000000000007105, -124.6807709998041531 ) ) ;
#6852 = ORIENTED_EDGE ( 'NONE', *, *, #1344, .F. ) ;
#6853 = EDGE_CURVE ( 'NONE', #4605, #8531, #9459, .T. ) ;
#6854 = AXIS2_PLACEMENT_3D ( 'NONE', #8674, #3964, #11386 ) ;
#6855 = EDGE_CURVE ( 'NONE', #6223, #9369, #6997, .T. ) ;
#6856 = CARTESIAN_POINT ( 'NONE',  ( 0.8038475772933666441, 10.39230484541326938, -2.501782431774985704E-16 ) ) ;
#6857 = FACE_BOUND ( 'NONE', #3918, .T. ) ;
#6858 = CARTESIAN_POINT ( 'NONE',  ( -1011.211222789229396, 114.9684118750914621, -141.4553492942763455 ) ) ;
#6859 = CARTESIAN_POINT ( 'NONE',  ( 20.71964524312746647, 180.2041921146487766, -123.3053720114591414 ) ) ;
#6860 = DIRECTION ( 'NONE',  ( 3.061276722312011504E-17, -1.000000000000000000, -0.000000000000000000 ) ) ;
#6861 = DIRECTION ( 'NONE',  ( 1.000000000000000000, 0.000000000000000000, 0.000000000000000000 ) ) ;
#6862 = EDGE_LOOP ( 'NONE', ( #10878, #9601 ) ) ;
#6863 = CARTESIAN_POINT ( 'NONE',  ( -951.4198147059590838, 125.0824040815807194, -126.6442663926291345 ) ) ;
#6864 = DIRECTION ( 'NONE',  ( 0.000000000000000000, 1.000000000000000000, 0.000000000000000000 ) ) ;
#6865 = CIRCLE ( 'NONE', #11214, 7.500000000000007105 ) ;
#6866 = TOROIDAL_SURFACE ( 'NONE', #4501, 4.000000000000045297, 1.000000000000000000 ) ;
#6867 = CARTESIAN_POINT ( 'NONE',  ( -27.99999999999999645, -6.000000000000000000, -27.99999999999999645 ) ) ;
#6868 = EDGE_LOOP ( 'NONE', ( #7680, #9790 ) ) ;
#6869 = ORIENTED_EDGE ( 'NONE', *, *, #11620, .F. ) ;
#6870 = CARTESIAN_POINT ( 'NONE',  ( 19.93152192967729519, 178.5613615780971202, -123.0243173142070816 ) ) ;
#6871 = CARTESIAN_POINT ( 'NONE',  ( -817.7441816825903516, 35.12288937987674586, -141.4553492942758908 ) ) ;
#6872 = CARTESIAN_POINT ( 'NONE',  ( -818.8285638327238303, 78.67432280806571043, -144.4023295390032899 ) ) ;
#6873 = AXIS2_PLACEMENT_3D ( 'NONE', #12062, #6190, #8962 ) ;
#6874 = CARTESIAN_POINT ( 'NONE',  ( -126.4213562373094959, 12.00000000000000000, 7.500000000000036415 ) ) ;
#6875 = DIRECTION ( 'NONE',  ( -0.000000000000000000, 1.000000000000000000, 7.930164461608263644E-17 ) ) ;
#6876 = CARTESIAN_POINT ( 'NONE',  ( -381.9362497754162291, 67.37496909217159669, -111.0233266882457173 ) ) ;
#6877 = CIRCLE ( 'NONE', #2524, 7.500000000000005329 ) ;
#6878 = VECTOR ( 'NONE', #7239, 1000.000000000000000 ) ;
#6879 = ORIENTED_EDGE ( 'NONE', *, *, #1844, .T. ) ;
#6880 = DIRECTION ( 'NONE',  ( -1.000000000000000000, 0.000000000000000000, 0.000000000000000000 ) ) ;
#6881 = CARTESIAN_POINT ( 'NONE',  ( -1021.607260580486013, 54.24386729702176524, -118.7903414690683661 ) ) ;
#6882 = CARTESIAN_POINT ( 'NONE',  ( -19.97026572922053944, 182.5268623749972505, -125.7890530056691745 ) ) ;
#6883 = CARTESIAN_POINT ( 'NONE',  ( -997.7839878466141954, 40.27522178589210711, -136.2353035311988378 ) ) ;
#6884 = AXIS2_PLACEMENT_3D ( 'NONE', #6113, #534, #1410 ) ;
#6885 = CARTESIAN_POINT ( 'NONE',  ( -382.3424684326698184, 95.66281168084425701, -110.0297798447839881 ) ) ;
#6886 = ORIENTED_EDGE ( 'NONE', *, *, #11356, .F. ) ;
#6887 = EDGE_LOOP ( 'NONE', ( #9537, #3861, #6809, #2934 ) ) ;
#6888 = CYLINDRICAL_SURFACE ( 'NONE', #8585, 7.500000000000007105 ) ;
#6889 = EDGE_CURVE ( 'NONE', #7831, #10076, #11496, .T. ) ;
#6890 = PRODUCT_CONTEXT ( 'NONE', #5496, 'mechanical' ) ;
#6891 = EDGE_LOOP ( 'NONE', ( #3815, #4662, #5509, #6194 ) ) ;
#6892 = CARTESIAN_POINT ( 'NONE',  ( -1028.581275045472694, 51.02622020309998163, -118.7903414690682240 ) ) ;
#6893 = DIRECTION ( 'NONE',  ( -1.000000000000000000, -0.000000000000000000, -0.000000000000000000 ) ) ;
#6894 =( GEOMETRIC_REPRESENTATION_CONTEXT ( 3 ) GLOBAL_UNCERTAINTY_ASSIGNED_CONTEXT ( ( #4974 ) ) GLOBAL_UNIT_ASSIGNED_CONTEXT ( ( #8426, #52, #3769 ) ) REPRESENTATION_CONTEXT ( 'NONE', 'WORKASPACE' ) );
#6895 = CARTESIAN_POINT ( 'NONE',  ( -822.7482738817717518, 104.4536172844453858, -103.3307627799637203 ) ) ;
#6896 = DIRECTION ( 'NONE',  ( 2.040851148208007875E-17, -1.000000000000000000, -0.000000000000000000 ) ) ;
#6897 = CARTESIAN_POINT ( 'NONE',  ( -20.00000000000008527, 177.7028087568835417, -124.7912233562835240 ) ) ;
#6898 = EDGE_LOOP ( 'NONE', ( #4384, #3906, #7268, #4001 ) ) ;
#6899 = AXIS2_PLACEMENT_3D ( 'NONE', #6772, #3937, #11479 ) ;
#6900 = EDGE_LOOP ( 'NONE', ( #1108, #9962, #11715, #7309 ) ) ;
#6901 = EDGE_CURVE ( 'NONE', #1936, #10559, #3427, .T. ) ;
#6903 = EDGE_CURVE ( 'NONE', #1611, #3186, #6607, .T. ) ;
#6902 = CARTESIAN_POINT ( 'NONE',  ( -1019.017691546883157, 99.44610047464911418, -96.78565065507929432 ) ) ;
#6904 = ORIENTED_EDGE ( 'NONE', *, *, #1187, .F. ) ;
#6905 = CARTESIAN_POINT ( 'NONE',  ( -1045.884592419587534, 115.0579440276406871, -130.5712005305406365 ) ) ;
#6906 = CARTESIAN_POINT ( 'NONE',  ( -926.5289067496701136, 125.3297071905304989, -130.5712005305407786 ) ) ;
#6907 = CYLINDRICAL_SURFACE ( 'NONE', #8671, 7.500000000000007994 ) ;
#6908 = DIRECTION ( 'NONE',  ( -0.3117078928809505767, -5.319854888938801199E-14, 0.9501779778103246477 ) ) ;
#6909 = ORIENTED_EDGE ( 'NONE', *, *, #2840, .T. ) ;
#6910 = DIRECTION ( 'NONE',  ( -1.000000000000000000, 0.000000000000000000, 0.000000000000000000 ) ) ;
#6911 = CARTESIAN_POINT ( 'NONE',  ( -822.2163178171774689, 83.41010758653600021, -104.7304854148471804 ) ) ;
#6912 = DIRECTION ( 'NONE',  ( 0.000000000000000000, 0.000000000000000000, 1.000000000000000000 ) ) ;
#6913 = DIRECTION ( 'NONE',  ( 0.000000000000000000, 0.000000000000000000, -1.000000000000000000 ) ) ;
#6914 = LINE ( 'NONE', #11563, #11163 ) ;
#6915 = ORIENTED_EDGE ( 'NONE', *, *, #5063, .F. ) ;
#6916 = CARTESIAN_POINT ( 'NONE',  ( 1.240837498110468453E-14, 12.00000000000001776, -126.4213562373094959 ) ) ;
#6917 = FACE_OUTER_BOUND ( 'NONE', #143, .T. ) ;
#6918 = EDGE_CURVE ( 'NONE', #6960, #8852, #8957, .T. ) ;
#6919 = LINE ( 'NONE', #11685, #10691 ) ;
#6920 = DIRECTION ( 'NONE',  ( 0.000000000000000000, 1.000000000000000000, 0.000000000000000000 ) ) ;
#6921 = EDGE_CURVE ( 'NONE', #8281, #9710, #2655, .T. ) ;
#6922 = CARTESIAN_POINT ( 'NONE',  ( 7.500000000000005329, 267.2792206135785591, -126.4213562373094959 ) ) ;
#6923 = VERTEX_POINT ( 'NONE', #9178 ) ;
#6924 =( REPRESENTATION_RELATIONSHIP ('NONE','NONE', #12149, #12068 ) REPRESENTATION_RELATIONSHIP_WITH_TRANSFORMATION ( #5549 )SHAPE_REPRESENTATION_RELATIONSHIP( ) );
#6925 = FACE_OUTER_BOUND ( 'NONE', #6983, .T. ) ;
#6926 = ORIENTED_EDGE ( 'NONE', *, *, #9644, .F. ) ;
#6927 = CARTESIAN_POINT ( 'NONE',  ( 19.98598762375597460, 179.0443862260074184, -123.7231531907395663 ) ) ;
#6928 = EDGE_CURVE ( 'NONE', #3899, #7054, #1397, .T. ) ;
#6929 = EDGE_CURVE ( 'NONE', #10270, #2780, #8244, .T. ) ;
#6930 = CARTESIAN_POINT ( 'NONE',  ( -819.4847856676407218, 76.17713329584785242, -105.5450962460541149 ) ) ;
#6931 = CARTESIAN_POINT ( 'NONE',  ( -1020.755281158171670, 68.40999151392655619, -149.7857175106638010 ) ) ;
#6932 = CARTESIAN_POINT ( 'NONE',  ( 0.000000000000000000, 0.000000000000000000, 0.000000000000000000 ) ) ;
#6933 = CARTESIAN_POINT ( 'NONE',  ( 0.07568653364057612021, -1.751902528125329539, -9.000000000000001776 ) ) ;
#6934 = CARTESIAN_POINT ( 'NONE',  ( -82.49999999999997158, 12.00000000000001421, -126.4213562373088564 ) ) ;
#6935 = CARTESIAN_POINT ( 'NONE',  ( -305.0000000000000568, 139.9999999999999716, -89.68077099980384048 ) ) ;
#6936 = EDGE_LOOP ( 'NONE', ( #9755, #10032 ) ) ;
#6937 = EDGE_CURVE ( 'NONE', #2015, #1342, #10942, .T. ) ;
#6938 = VERTEX_POINT ( 'NONE', #7142 ) ;
#6939 = AXIS2_PLACEMENT_3D ( 'NONE', #10539, #208, #3993 ) ;
#6940 = CARTESIAN_POINT ( 'NONE',  ( -957.1839320239914741, 48.17551948191501765, -118.7903414690682951 ) ) ;
#6941 = PLANE ( 'NONE',  #5474 ) ;
#6942 = FACE_OUTER_BOUND ( 'NONE', #3298, .T. ) ;
#6943 = CARTESIAN_POINT ( 'NONE',  ( -957.0819499390250940, 50.45265437475578807, -136.2353035311988663 ) ) ;
#6944 = ORIENTED_EDGE ( 'NONE', *, *, #10601, .F. ) ;
#6945 = DIRECTION ( 'NONE',  ( -0.7071067811865479058, 0.000000000000000000, -0.7071067811865472397 ) ) ;
#6946 = ORIENTED_EDGE ( 'NONE', *, *, #11769, .T. ) ;
#6947 = DIRECTION ( 'NONE',  ( 0.000000000000000000, 1.000000000000000000, 0.000000000000000000 ) ) ;
#6948 = EDGE_LOOP ( 'NONE', ( #9662, #10026, #1154 ) ) ;
#6949 = CONTEXT_DEPENDENT_SHAPE_REPRESENTATION ( #3589, #5848 ) ;
#6950 = VERTEX_POINT ( 'NONE', #10970 ) ;
#6951 = VECTOR ( 'NONE', #11918, 999.9999999999998863 ) ;
#6952 = CARTESIAN_POINT ( 'NONE',  ( -1048.438004920982848, 39.66697241395321782, -126.6442663926296603 ) ) ;
#6953 = CARTESIAN_POINT ( 'NONE',  ( -270.0000000000000000, 12.00000000000001066, -126.4213562373076059 ) ) ;
#6954 = LINE ( 'NONE', #2949, #3202 ) ;
#6955 = UNCERTAINTY_MEASURE_WITH_UNIT (LENGTH_MEASURE( 1.000000000000000082E-05 ), #1676, 'distance_accuracy_value', 'NONE');
#6956 = CARTESIAN_POINT ( 'NONE',  ( -1055.469533842434430, 91.91071092603658599, -96.78565065507918064 ) ) ;
#6957 = CARTESIAN_POINT ( 'NONE',  ( 4.808665244885994618E-14, -6.000000000000000000, 141.4213562373094817 ) ) ;
#6958 = CARTESIAN_POINT ( 'NONE',  ( -240.0000000000000000, 12.00000000000001066, -126.4213562373078190 ) ) ;
#6959 = AXIS2_PLACEMENT_3D ( 'NONE', #9905, #9786, #1439 ) ;
#6960 = VERTEX_POINT ( 'NONE', #10906 ) ;
#6961 = EDGE_LOOP ( 'NONE', ( #189, #10780 ) ) ;
#6962 = CARTESIAN_POINT ( 'NONE',  ( -1025.595388641369482, 103.7168792382126128, -99.57582448894517313 ) ) ;
#6963 = CARTESIAN_POINT ( 'NONE',  ( -1021.777026427250121, 118.8177985574659346, -130.5712005305405228 ) ) ;
#6964 = CARTESIAN_POINT ( 'NONE',  ( -1024.691966601151762, 118.8493250655917564, -126.6442663926291061 ) ) ;
#6965 = CARTESIAN_POINT ( 'NONE',  ( -60.00000000000000000, 139.9999999999999716, -126.4213562373090696 ) ) ;
#6966 = CARTESIAN_POINT ( 'NONE',  ( 3.133148353965215262E-13, 12.00000000000000000, -103.9213562373094959 ) ) ;
#6967 = EDGE_CURVE ( 'NONE', #1856, #3561, #8185, .T. ) ;
#6968 = ORIENTED_EDGE ( 'NONE', *, *, #6083, .T. ) ;
#6969 = EDGE_CURVE ( 'NONE', #4621, #7284, #8397, .T. ) ;
#6970 = AXIS2_PLACEMENT_3D ( 'NONE', #9256, #5609, #9385 ) ;
#6971 = FACE_BOUND ( 'NONE', #11257, .T. ) ;
#6972 = CARTESIAN_POINT ( 'NONE',  ( -1014.132585063772581, 52.13780504951625261, -124.6807709998041531 ) ) ;
#6973 = CARTESIAN_POINT ( 'NONE',  ( -370.8011028251392531, 105.8825848193712460, -112.1920252379657796 ) ) ;
#6974 = CARTESIAN_POINT ( 'NONE',  ( 20.89912381907808125, 178.8409046240913085, -124.1420537659444534 ) ) ;
#6975 = ORIENTED_EDGE ( 'NONE', *, *, #4276, .T. ) ;
#6976 = DIRECTION ( 'NONE',  ( -8.163404592832030268E-17, 1.000000000000000000, -0.000000000000000000 ) ) ;
#6977 = CARTESIAN_POINT ( 'NONE',  ( -974.1288507787422759, 124.2142274477005657, -124.6807709998040110 ) ) ;
#6978 = ADVANCED_FACE ( 'NONE', ( #2561 ), #8132, .F. ) ;
#6979 = CARTESIAN_POINT ( 'NONE',  ( 1.561981751485805177E-12, -6.000000000000005329, 23.57864376269050410 ) ) ;
#6980 = CARTESIAN_POINT ( 'NONE',  ( -374.9097930543319421, 78.37721037988610817, -94.95651375212828782 ) ) ;
#6981 = AXIS2_PLACEMENT_3D ( 'NONE', #369, #4150, #2356 ) ;
#6982 = DIRECTION ( 'NONE',  ( -0.000000000000000000, 1.000000000000000000, 7.930164461608263644E-17 ) ) ;
#6983 = EDGE_LOOP ( 'NONE', ( #9110, #716, #9721 ) ) ;
#6984 = CARTESIAN_POINT ( 'NONE',  ( -380.5583952655373992, 64.47352604413475774, -134.3328398924245448 ) ) ;
#6985 = CARTESIAN_POINT ( 'NONE',  ( -1061.884876827093876, 80.20192378191431715, -154.8742214401230797 ) ) ;
#6986 = CIRCLE ( 'NONE', #1273, 7.500000000000008882 ) ;
#6987 = ADVANCED_FACE ( 'NONE', ( #9985, #4305 ), #11896, .F. ) ;
#6988 = CIRCLE ( 'NONE', #9571, 175.0000000000000000 ) ;
#6989 = CARTESIAN_POINT ( 'NONE',  ( 0.000000000000000000, 12.00000000000001776, -124.6807709998038405 ) ) ;
#6990 = DIRECTION ( 'NONE',  ( 0.000000000000000000, 0.000000000000000000, 1.000000000000000000 ) ) ;
#6991 = CARTESIAN_POINT ( 'NONE',  ( -151.3258811035894098, 0.000000000000000000, -56.13263083939680342 ) ) ;
#6992 = DIRECTION ( 'NONE',  ( -0.7071067811865473507, -0.000000000000000000, 0.7071067811865477948 ) ) ;
#6993 = DIRECTION ( 'NONE',  ( 1.000000000000000000, 0.000000000000000000, 0.000000000000000000 ) ) ;
#6994 = ORIENTED_EDGE ( 'NONE', *, *, #4752, .T. ) ;
#6995 = CARTESIAN_POINT ( 'NONE',  ( -1057.521967982373098, 48.25222617153974625, -141.4553492942758623 ) ) ;
#6996 = EDGE_LOOP ( 'NONE', ( #5636, #6218, #1516, #9406 ) ) ;
#6997 = CIRCLE ( 'NONE', #5406, 7.500000000000007105 ) ;
#6998 = CIRCLE ( 'NONE', #1671, 20.00000000000000000 ) ;
#6999 = DIRECTION ( 'NONE',  ( 0.000000000000000000, -0.5000000000000009992, 0.8660254037844380415 ) ) ;
#7000 = CARTESIAN_POINT ( 'NONE',  ( -1032.658196452834773, 44.72920460984212809, -122.7172756069792143 ) ) ;
#7001 = EDGE_LOOP ( 'NONE', ( #5073, #10412 ) ) ;
#7002 = EDGE_CURVE ( 'NONE', #12185, #20, #9953, .T. ) ;
#7003 = CARTESIAN_POINT ( 'NONE',  ( -154.5043356068770493, 0.000000000000000000, -94.56666130601601594 ) ) ;
#7004 = CARTESIAN_POINT ( 'NONE',  ( 8.937118865183856033E-16, 196.0000000000000000, -124.6807709998038405 ) ) ;
#7005 = CARTESIAN_POINT ( 'NONE',  ( -822.2158551983004600, 73.93035145837139055, -154.6498254730319957 ) ) ;
#7006 = EDGE_LOOP ( 'NONE', ( #7931, #3146 ) ) ;
#7007 = AXIS2_PLACEMENT_3D ( 'NONE', #10223, #10160, #3469 ) ;
#7008 = ORIENTED_EDGE ( 'NONE', *, *, #3828, .F. ) ;
#7009 = CARTESIAN_POINT ( 'NONE',  ( -1028.611899521407167, 50.57492120214475761, -126.6442663926292340 ) ) ;
#7010 = CARTESIAN_POINT ( 'NONE',  ( 20.00000000000000355, 177.7115707886026144, -124.6807709998038547 ) ) ;
#7011 = DIRECTION ( 'NONE',  ( 0.000000000000000000, 0.000000000000000000, 1.000000000000000000 ) ) ;
#7012 = CARTESIAN_POINT ( 'NONE',  ( -828.8285638327243987, 78.67432280806561096, -104.9592124606052863 ) ) ;
#7013 = CARTESIAN_POINT ( 'NONE',  ( 141.4213562373095101, -6.000000000000000000, -1.508194112741312283E-14 ) ) ;
#7014 = COLOUR_RGB ( '', 0.40784314, 0.44705882, 0.49803922) ;
#7015 = CARTESIAN_POINT ( 'NONE',  ( -1011.935294340108044, 99.50314415908297860, -96.78565065507922327 ) ) ;
#7016 = CARTESIAN_POINT ( 'NONE',  ( -925.0000000000000000, 81.99999999999988631, -124.6807709998038405 ) ) ;
#7017 = EDGE_LOOP ( 'NONE', ( #8099, #4002, #2364, #12136 ) ) ;
#7018 = CYLINDRICAL_SURFACE ( 'NONE', #9552, 7.500000000000005329 ) ;
#7019 = CARTESIAN_POINT ( 'NONE',  ( -370.5475656004942380, 57.43166175920264038, -114.0709556960625406 ) ) ;
#7020 = VERTEX_POINT ( 'NONE', #10046 ) ;
#7021 = CARTESIAN_POINT ( 'NONE',  ( -820.5239792770877330, 82.44072200957887731, -154.2973869372356432 ) ) ;
#7022 = CARTESIAN_POINT ( 'NONE',  ( -954.7734463792770612, 107.7731650919851205, -99.57582448894495997 ) ) ;
#7023 = CYLINDRICAL_SURFACE ( 'NONE', #1162, 1.500000000000000444 ) ;
#7024 = CARTESIAN_POINT ( 'NONE',  ( -1037.337636019037518, 116.9882293220590270, -126.6442663926289640 ) ) ;
#7025 = DIRECTION ( 'NONE',  ( 0.000000000000000000, 0.000000000000000000, -1.000000000000000000 ) ) ;
#7026 = DIRECTION ( 'NONE',  ( -1.000000000000000000, 0.000000000000000000, 0.000000000000000000 ) ) ;
#7027 = CARTESIAN_POINT ( 'NONE',  ( -1017.840614713424657, 119.3387310954205986, -118.7903414690676556 ) ) ;
#7028 = DIRECTION ( 'NONE',  ( 2.040851148208007875E-17, -1.000000000000000000, -0.000000000000000000 ) ) ;
#7029 = CARTESIAN_POINT ( 'NONE',  ( -19.98684882777175531, 182.5205802027333277, -123.9330515924332161 ) ) ;
#7030 = DIRECTION ( 'NONE',  ( -0.9501779778103371932, 0.000000000000000000, 0.3117078928809124960 ) ) ;
#7031 = FACE_BOUND ( 'NONE', #3840, .T. ) ;
#7032 = CYLINDRICAL_SURFACE ( 'NONE', #3730, 7.500000000000007105 ) ;
#7033 = CIRCLE ( 'NONE', #1715, 7.500000000000007105 ) ;
#7034 = CARTESIAN_POINT ( 'NONE',  ( -818.9564113685823941, 79.80952029794852365, -94.80345787799255675 ) ) ;
#7035 = VERTEX_POINT ( 'NONE', #11961 ) ;
#7036 = DIRECTION ( 'NONE',  ( -0.000000000000000000, 1.000000000000000000, -0.000000000000000000 ) ) ;
#7037 = DIRECTION ( 'NONE',  ( 0.000000000000000000, -0.4999999999999995004, 0.8660254037844389297 ) ) ;
#7038 = EDGE_CURVE ( 'NONE', #1615, #1810, #2264, .T. ) ;
#7039 = DIRECTION ( 'NONE',  ( 1.000000000000000000, 0.000000000000000000, 0.000000000000000000 ) ) ;
#7040 = CARTESIAN_POINT ( 'NONE',  ( -374.1184086109046802, 70.90605591669974217, -97.47965622763319971 ) ) ;
#7041 = FACE_OUTER_BOUND ( 'NONE', #2186, .T. ) ;
#7042 = VERTEX_POINT ( 'NONE', #5397 ) ;
#7043 = ORIENTED_EDGE ( 'NONE', *, *, #3501, .T. ) ;
#7044 = CARTESIAN_POINT ( 'NONE',  ( -380.0144971365231754, 63.46555453814624315, -132.2185027065989686 ) ) ;
#7045 = CARTESIAN_POINT ( 'NONE',  ( -372.1715096098437243, 101.7023887269710229, -144.5189483497782987 ) ) ;
#7046 = CARTESIAN_POINT ( 'NONE',  ( -180.0000000000000000, 12.00000000000001421, -126.4213562373082453 ) ) ;
#7047 = AXIS2_PLACEMENT_3D ( 'NONE', #5630, #5566, #4656 ) ;
#7048 = DIRECTION ( 'NONE',  ( -0.000000000000000000, 1.000000000000000000, 7.930164461608263644E-17 ) ) ;
#7049 =( NAMED_UNIT ( * ) PLANE_ANGLE_UNIT ( ) SI_UNIT ( $, .RADIAN. ) );
#7050 = DIRECTION ( 'NONE',  ( -0.000000000000000000, -1.000000000000000000, -0.000000000000000000 ) ) ;
#7051 = ORIENTED_EDGE ( 'NONE', *, *, #6889, .T. ) ;
#7052 = CARTESIAN_POINT ( 'NONE',  ( -1057.299536696276846, 52.76571712355565325, -146.0307792196449554 ) ) ;
#7053 = ADVANCED_FACE ( 'NONE', ( #11165, #10352, #6585, #4554, #12218, #1895, #7570, #3741, #3538, #10236 ), #8265, .F. ) ;
#7054 = VERTEX_POINT ( 'NONE', #968 ) ;
#7055 = B_SPLINE_CURVE_WITH_KNOTS ( 'NONE', 3,
 ( #2531, #1801, #7361, #1604, #880, #746, #816, #5563 ),
 .UNSPECIFIED., .F., .F.,
 ( 4, 2, 2, 4 ),
 ( 0.005257893453559901037, 0.006567392922673234712, 0.007876892391786568387, 0.01049589133001323574 ),
 .UNSPECIFIED. ) ;
#7056 = ORIENTED_EDGE ( 'NONE', *, *, #5656, .F. ) ;
#7057 = DIRECTION ( 'NONE',  ( 0.000000000000000000, 1.000000000000000000, -0.000000000000000000 ) ) ;
#7058 = CARTESIAN_POINT ( 'NONE',  ( -795.0000000000061391, 52.38665522077228331, -118.7903414690680250 ) ) ;
#7059 = ORIENTED_EDGE ( 'NONE', *, *, #12118, .T. ) ;
#7060 = DIRECTION ( 'NONE',  ( 0.000000000000000000, 1.000000000000000000, 0.000000000000000000 ) ) ;
#7061 = CARTESIAN_POINT ( 'NONE',  ( 1.562900236585165577E-12, 0.000000000000000000, 16.07864376269049700 ) ) ;
#7062 = ORIENTED_EDGE ( 'NONE', *, *, #635, .F. ) ;
#7063 = CIRCLE ( 'NONE', #3915, 7.500000000000007105 ) ;
#7064 = ADVANCED_BREP_SHAPE_REPRESENTATION ( '', ( #8008, #11957 ), #9978 ) ;
#7065 = ORIENTED_EDGE ( 'NONE', *, *, #6240, .F. ) ;
#7066 = VECTOR ( 'NONE', #10864, 1000.000000000000000 ) ;
#7067 = LINE ( 'NONE', #1506, #9963 ) ;
#7068 = EDGE_CURVE ( 'NONE', #818, #10791, #11779, .T. ) ;
#7069 = EDGE_CURVE ( 'NONE', #4581, #6347, #1703, .T. ) ;
#7070 = AXIS2_PLACEMENT_3D ( 'NONE', #5679, #10316, #1858 ) ;
#7071 = CARTESIAN_POINT ( 'NONE',  ( -795.0000000000079581, 93.55451860843940892, -96.78565065507920906 ) ) ;
#7072 = CARTESIAN_POINT ( 'NONE',  ( -19.88795444598854445, 178.6948919461029561, -126.7979262391024946 ) ) ;
#7073 = VECTOR ( 'NONE', #4927, 1000.000000000000000 ) ;
#7074 = ADVANCED_FACE ( 'NONE', ( #5464 ), #8459, .F. ) ;
#7075 = ORIENTED_EDGE ( 'NONE', *, *, #2976, .T. ) ;
#7076 = DIRECTION ( 'NONE',  ( -1.000000000000000000, 0.000000000000000000, 0.000000000000000000 ) ) ;
#7077 =( LENGTH_UNIT ( ) NAMED_UNIT ( * ) SI_UNIT ( .MILLI., .METRE. ) );
#7078 = ORIENTED_EDGE ( 'NONE', *, *, #11470, .T. ) ;
#7079 = CARTESIAN_POINT ( 'NONE',  ( -21.02742354149708603, 178.6868688154197002, -125.1152650341464891 ) ) ;
#7080 = CIRCLE ( 'NONE', #568, 7.500000000000020428 ) ;
#7081 = CARTESIAN_POINT ( 'NONE',  ( 0.000000000000000000, -58.00000000000000711, -126.4213562373094959 ) ) ;
#7082 = ORIENTED_EDGE ( 'NONE', *, *, #10228, .T. ) ;
#7083 = CARTESIAN_POINT ( 'NONE',  ( -955.6263874535618470, 86.32439835342511003, -94.48732055948597974 ) ) ;
#7084 = CARTESIAN_POINT ( 'NONE',  ( -45.53315400109751465, 12.00000000000000000, -237.8419396193594650 ) ) ;
#7085 = CLOSED_SHELL ( 'NONE', ( #7655, #1780, #6634, #1634, #4424, #975, #1592, #10297, #9276, #9329, #4579 ) ) ;
#7086 = CARTESIAN_POINT ( 'NONE',  ( -21.05658410469665043, 181.5474309616008952, -125.5905239331273862 ) ) ;
#7087 = EDGE_CURVE ( 'NONE', #8092, #6181, #680, .T. ) ;
#7088 = FACE_OUTER_BOUND ( 'NONE', #8787, .T. ) ;
#7089 = CARTESIAN_POINT ( 'NONE',  ( 4.808665244885994618E-14, 0.000000000000000000, 141.4213562373094817 ) ) ;
#7090 = DIRECTION ( 'NONE',  ( 0.000000000000000000, 1.000000000000000000, 0.000000000000000000 ) ) ;
#7091 = AXIS2_PLACEMENT_3D ( 'NONE', #3825, #741, #4519 ) ;
#7092 = CIRCLE ( 'NONE', #1777, 7.500000000000007105 ) ;
#7093 = CARTESIAN_POINT ( 'NONE',  ( -828.6703486388499869, 79.96407734986385663, -104.7820573548426069 ) ) ;
#7094 = CARTESIAN_POINT ( 'NONE',  ( -901.8785362142588156, 56.55314031071017666, -124.6807709998039968 ) ) ;
#7095 = CIRCLE ( 'NONE', #5916, 7.500000000000007105 ) ;
#7096 = CARTESIAN_POINT ( 'NONE',  ( -819.3351944727438649, 80.89172441788861079, -94.89089580185901696 ) ) ;
#7097 = FACE_OUTER_BOUND ( 'NONE', #4169, .T. ) ;
#7098 = EDGE_LOOP ( 'NONE', ( #1793, #9612, #2176, #2956, #11314 ) ) ;
#7099 = LINE ( 'NONE', #9884, #2714 ) ;
#7100 = CARTESIAN_POINT ( 'NONE',  ( -954.0441199534440102, 124.9954171138387977, -124.6807709998039115 ) ) ;
#7101 = DIRECTION ( 'NONE',  ( -0.000000000000000000, -0.000000000000000000, -1.000000000000000000 ) ) ;
#7102 = CARTESIAN_POINT ( 'NONE',  ( -375.0000000000000568, 82.00000000000093792, -94.68077099980381206 ) ) ;
#7103 = CARTESIAN_POINT ( 'NONE',  ( -374.7780441258248061, 76.25198850915256799, -95.36283402834658318 ) ) ;
#7104 = CARTESIAN_POINT ( 'NONE',  ( 30.00000000000000000, -6.000000000000000000, -30.00000000000000000 ) ) ;
#7105 = ORIENTED_EDGE ( 'NONE', *, *, #651, .F. ) ;
#7106 = EDGE_LOOP ( 'NONE', ( #10294, #10262, #5913, #7390 ) ) ;
#7107 = CARTESIAN_POINT ( 'NONE',  ( -383.0048299740013249, 70.12786572434940524, -140.8172186891583237 ) ) ;
#7108 = CARTESIAN_POINT ( 'NONE',  ( -1012.828629370413182, 79.69572830938452057, -154.2940595301284361 ) ) ;
#7109 = CARTESIAN_POINT ( 'NONE',  ( -828.6674387974398996, 77.37343372931326257, -144.1410586993683012 ) ) ;
#7110 = CARTESIAN_POINT ( 'NONE',  ( -370.7831763668500571, 105.9365648485286471, -137.0819547014295097 ) ) ;
#7111 = CARTESIAN_POINT ( 'NONE',  ( -45.53315400109751465, 0.000000000000000000, -230.3419396193594366 ) ) ;
#7112 = CARTESIAN_POINT ( 'NONE',  ( -827.8046876470999678, 75.62493715853115361, -94.68085105088540843 ) ) ;
#7113 = FACE_OUTER_BOUND ( 'NONE', #11007, .T. ) ;
#7114 = B_SPLINE_CURVE_WITH_KNOTS ( 'NONE', 3,
 ( #9170, #8451, #12085, #4612, #7383, #2681, #6453, #641 ),
 .UNSPECIFIED., .F., .F.,
 ( 4, 2, 2, 4 ),
 ( 0.005257893453559908843, 0.006567392922673242518, 0.007876892391786575326, 0.01049589133001324094 ),
 .UNSPECIFIED. ) ;
#7115 = CARTESIAN_POINT ( 'NONE',  ( 120.8820948793965186, 12.00000000000000000, -186.6989091883332890 ) ) ;
#7116 = VERTEX_POINT ( 'NONE', #204 ) ;
#7117 = CARTESIAN_POINT ( 'NONE',  ( -953.8433812051875975, 65.95343150956774991, -149.7857175106634315 ) ) ;
#7118 = ORIENTED_EDGE ( 'NONE', *, *, #3820, .T. ) ;
#7119 = VERTEX_POINT ( 'NONE', #11530 ) ;
#7120 = ADVANCED_FACE ( 'NONE', ( #5902 ), #6888, .F. ) ;
#7121 = CARTESIAN_POINT ( 'NONE',  ( 1.250503886288004501E-12, 152.0000000000000000, -13.92135623730949234 ) ) ;
#7122 = CARTESIAN_POINT ( 'NONE',  ( -19.91081574664475795, 181.5182364730088125, -122.7941294590836492 ) ) ;
#7123 = EDGE_CURVE ( 'NONE', #1455, #9404, #5614, .T. ) ;
#7124 = ORIENTED_EDGE ( 'NONE', *, *, #7068, .F. ) ;
#7125 = CYLINDRICAL_SURFACE ( 'NONE', #5364, 7.500000000000007994 ) ;
#7126 = ORIENTED_EDGE ( 'NONE', *, *, #2976, .F. ) ;
#7127 = AXIS2_PLACEMENT_3D ( 'NONE', #7950, #11722, #3237 ) ;
#7128 = ORIENTED_EDGE ( 'NONE', *, *, #3655, .T. ) ;
#7129 = EDGE_CURVE ( 'NONE', #2078, #3022, #3238, .T. ) ;
#7130 = LINE ( 'NONE', #8064, #9373 ) ;
#7131 = VECTOR ( 'NONE', #7150, 1000.000000000000000 ) ;
#7132 = CARTESIAN_POINT ( 'NONE',  ( -6.203669305690495683E-15, 7.351593252548062729, 5.266666970006212978 ) ) ;
#7133 = CARTESIAN_POINT ( 'NONE',  ( -1065.000000000005912, 82.00000000000039790, -94.48732055948609343 ) ) ;
#7134 = CARTESIAN_POINT ( 'NONE',  ( 0.000000000000000000, 139.9999999999999716, -124.6807709998038405 ) ) ;
#7135 = CARTESIAN_POINT ( 'NONE',  ( -925.0000000000000000, 61.99999999999980815, -124.6807709998038405 ) ) ;
#7136 = CARTESIAN_POINT ( 'NONE',  ( -374.9726451943776055, 84.25168756434180750, -94.76384896039375860 ) ) ;
#7137 = ORIENTED_EDGE ( 'NONE', *, *, #4752, .F. ) ;
#7138 = FACE_OUTER_BOUND ( 'NONE', #328, .T. ) ;
#7139 = CARTESIAN_POINT ( 'NONE',  ( -379.9115039592767857, 63.28126683224602544, -117.6075586578124046 ) ) ;
#7140 = AXIS2_PLACEMENT_3D ( 'NONE', #11175, #8275, #10916 ) ;
#7141 = ORIENTED_EDGE ( 'NONE', *, *, #7686, .T. ) ;
#7142 = CARTESIAN_POINT ( 'NONE',  ( 7.653191805780027529E-16, 138.9999999999999716, -81.42135623730948168 ) ) ;
#7143 = ADVANCED_FACE ( 'NONE', ( #4505 ), #5289, .F. ) ;
#7144 = DIRECTION ( 'NONE',  ( 0.7071067811865473507, 0.000000000000000000, -0.7071067811865477948 ) ) ;
#7145 = ORIENTED_EDGE ( 'NONE', *, *, #9458, .F. ) ;
#7146 = CARTESIAN_POINT ( 'NONE',  ( -820.4595805503671500, 72.64106675864344709, -94.48732055948583763 ) ) ;
#7147 = CARTESIAN_POINT ( 'NONE',  ( 9.796085511398436814E-16, 152.0000000000000000, -126.4213562373094959 ) ) ;
#7148 = CARTESIAN_POINT ( 'NONE',  ( -1010.922847972424620, 120.6260792194949829, -126.6442663926288503 ) ) ;
#7149 = PRODUCT_DEFINITION ( 'UNKNOWN', '', #9202, #3808 ) ;
#7150 = DIRECTION ( 'NONE',  ( 0.000000000000000000, 1.000000000000000000, 0.000000000000000000 ) ) ;
#7151 = CIRCLE ( 'NONE', #8736, 20.00000000000008882 ) ;
#7152 = CARTESIAN_POINT ( 'NONE',  ( -1060.846413679908210, 110.5345601522217720, -113.1262384684099374 ) ) ;
#7153 = DIRECTION ( 'NONE',  ( -0.000000000000000000, -0.000000000000000000, -1.000000000000000000 ) ) ;
#7154 = CARTESIAN_POINT ( 'NONE',  ( -819.4840074578143003, 76.17856360854463560, -143.8168744253322870 ) ) ;
#7155 = FACE_BOUND ( 'NONE', #11565, .T. ) ;
#7156 = CARTESIAN_POINT ( 'NONE',  ( 144.0488662551573782, 0.000000000000000000, -146.9077238332702109 ) ) ;
#7157 = CARTESIAN_POINT ( 'NONE',  ( 0.000000000000000000, 24.00000000000001776, -124.6807709998038405 ) ) ;
#7158 = APPLICATION_CONTEXT ( 'automotive_design' ) ;
#7159 = ADVANCED_FACE ( 'NONE', ( #9066 ), #6346, .F. ) ;
#7160 = EDGE_LOOP ( 'NONE', ( #263, #4905, #1027, #4930, #2466 ) ) ;
#7161 = FACE_OUTER_BOUND ( 'NONE', #5551, .T. ) ;
#7162 = CARTESIAN_POINT ( 'NONE',  ( -954.0688428831313104, 124.4732772249355577, -118.7903414690677693 ) ) ;
#7163 = DIRECTION ( 'NONE',  ( 0.000000000000000000, -0.5000000000000009992, 0.8660254037844380415 ) ) ;
#7164 = LINE ( 'NONE', #4324, #7066 ) ;
#7165 = CARTESIAN_POINT ( 'NONE',  ( -217.5000000000000000, 12.00000000000001421, -126.4213562373080180 ) ) ;
#7166 = DIRECTION ( 'NONE',  ( 0.000000000000000000, 0.000000000000000000, 1.000000000000000000 ) ) ;
#7167 = EDGE_LOOP ( 'NONE', ( #10598, #10146 ) ) ;
#7168 = AXIS2_PLACEMENT_3D ( 'NONE', #10685, #5989, #9758 ) ;
#7169 = ORIENTED_EDGE ( 'NONE', *, *, #9320, .F. ) ;
#7170 = CARTESIAN_POINT ( 'NONE',  ( 19.88620277217341936, 179.4101426937791075, -122.5498900800241415 ) ) ;
#7171 = CARTESIAN_POINT ( 'NONE',  ( -19.92079578072784329, 178.7178626825727576, -122.8973188108788150 ) ) ;
#7172 = CARTESIAN_POINT ( 'NONE',  ( -823.4903519156995344, 73.67469885889941850, -142.8656372648663080 ) ) ;
#7173 = CARTESIAN_POINT ( 'NONE',  ( -819.8285638327238303, 78.67432280806536937, -89.68077099980398259 ) ) ;
#7174 = CYLINDRICAL_SURFACE ( 'NONE', #9155, 20.00000000000000000 ) ;
#7175 = CARTESIAN_POINT ( 'NONE',  ( 1.387778780781445676E-14, -58.00000000000000711, 126.4213562373094959 ) ) ;
#7176 = CYLINDRICAL_SURFACE ( 'NONE', #11243, 7.500000000000007105 ) ;
#7177 = AXIS2_PLACEMENT_3D ( 'NONE', #4979, #279, #4067 ) ;
#7178 = DIRECTION ( 'NONE',  ( -8.163404592832030268E-17, 1.000000000000000000, -0.000000000000000000 ) ) ;
#7179 = EDGE_LOOP ( 'NONE', ( #6021, #2635, #10067, #2914 ) ) ;
#7180 = CARTESIAN_POINT ( 'NONE',  ( -1028.259718048100012, 56.21337363619606720, -141.4553492942759476 ) ) ;
#7181 = VERTEX_POINT ( 'NONE', #1724 ) ;
#7182 = CARTESIAN_POINT ( 'NONE',  ( -120.0000000000000000, 152.0000000000000000, -126.4213562373086575 ) ) ;
#7183 = AXIS2_PLACEMENT_3D ( 'NONE', #3429, #11110, #10054 ) ;
#7184 = AXIS2_PLACEMENT_3D ( 'NONE', #7486, #11067, #2592 ) ;
#7185 = DIRECTION ( 'NONE',  ( -0.000000000000000000, 1.000000000000000000, -0.000000000000000000 ) ) ;
#7186 = EDGE_LOOP ( 'NONE', ( #1822, #5516, #12129, #9492 ) ) ;
#7187 = CARTESIAN_POINT ( 'NONE',  ( -379.7921418149325063, 63.07164944986214294, -118.2218589047913468 ) ) ;
#7188 = CARTESIAN_POINT ( 'NONE',  ( -379.4171904840047205, 101.5744813863694134, -120.5347007855791617 ) ) ;
#7189 = ORIENTED_EDGE ( 'NONE', *, *, #7970, .T. ) ;
#7190 = CIRCLE ( 'NONE', #6605, 7.500000000000012434 ) ;
#7191 = EDGE_CURVE ( 'NONE', #10332, #6347, #1470, .T. ) ;
#7192 = CIRCLE ( 'NONE', #10158, 7.500000000000007105 ) ;
#7193 = AXIS2_PLACEMENT_3D ( 'NONE', #2738, #6506, #2116 ) ;
#7194 = FACE_OUTER_BOUND ( 'NONE', #3603, .T. ) ;
#7195 = EDGE_CURVE ( 'NONE', #5919, #9092, #12224, .T. ) ;
#7196 = CARTESIAN_POINT ( 'NONE',  ( 2.186774452080127126E-12, -6.000000000000005329, 83.57864376269050410 ) ) ;
#7197 = CARTESIAN_POINT ( 'NONE',  ( -1019.365209469143679, 93.24061105504411273, -95.06748246948018277 ) ) ;
#7198 = FACE_OUTER_BOUND ( 'NONE', #6584, .T. ) ;
#7199 = DIRECTION ( 'NONE',  ( -3.061276722312011504E-17, 1.000000000000000000, 0.000000000000000000 ) ) ;
#7200 = VECTOR ( 'NONE', #2977, 1000.000000000000000 ) ;
#7201 = CONICAL_SURFACE ( 'NONE', #5625, 9.000000000000000000, 1.047197551196600296 ) ;
#7202 =( NAMED_UNIT ( * ) PLANE_ANGLE_UNIT ( ) SI_UNIT ( $, .RADIAN. ) );
#7203 = ORIENTED_EDGE ( 'NONE', *, *, #2069, .F. ) ;
#7204 = CARTESIAN_POINT ( 'NONE',  ( 8.937118865183852088E-16, 196.0000000000000000, -124.6807709998038405 ) ) ;
#7205 =( LENGTH_UNIT ( ) NAMED_UNIT ( * ) SI_UNIT ( .MILLI., .METRE. ) );
#7206 = CARTESIAN_POINT ( 'NONE',  ( 1.561981751485805177E-12, 12.00000000000000000, 31.07864376269051121 ) ) ;
#7207 = VERTEX_POINT ( 'NONE', #11468 ) ;
#7208 = CARTESIAN_POINT ( 'NONE',  ( -823.1748664167885181, 83.64213179714484170, -154.1150047552051490 ) ) ;
#7209 = DIRECTION ( 'NONE',  ( 0.000000000000000000, 1.000000000000000000, 0.000000000000000000 ) ) ;
#7210 = CARTESIAN_POINT ( 'NONE',  ( -991.5701548301636876, 122.8678427087060214, -124.6807709998040536 ) ) ;
#7211 = B_SPLINE_CURVE_WITH_KNOTS ( 'NONE', 3,
 ( #4936, #4194, #7972, #7034, #10804, #2344, #11798, #7096, #3314, #6115, #10859, #9882, #5174, #5230, #9002, #9936, #1472, #4317, #535, #432, #5144, #4164, #4222, #9726, #11770, #8905, #4291, #8974, #7938, #499, #11829, #8000, #10888, #9784, #4109, #9030, #11711, #570, #3286, #3224 ),
 .UNSPECIFIED., .F., .F.,
 ( 4, 2, 2, 2, 2, 2, 2, 2, 2, 2, 2, 2, 2, 2, 2, 2, 2, 2, 2, 4 ),
 ( 0.000000000000000000, 0.0009792129545681763775, 0.001468819431852298393, 0.001958425909136420843, 0.002937638863704576404, 0.003916851818272732398, 0.004896064772840888826, 0.005875277727409044387, 0.006854490681977199081, 0.007833703636545355509, 0.008812916591113511069, 0.009792129545681668365, 0.01028173602296574528, 0.01077134250024982393, 0.01175055545481823276, 0.01272976840938664506, 0.01321937488667085207, 0.01370898136395505736, 0.01468819431852334649, 0.01566740727309163389 ),
 .UNSPECIFIED. ) ;
#7212 = EDGE_CURVE ( 'NONE', #2514, #11133, #5202, .T. ) ;
#7213 = PRESENTATION_LAYER_ASSIGNMENT (  '', '', ( #3255 ) ) ;
#7214 = EDGE_CURVE ( 'NONE', #609, #5232, #7192, .T. ) ;
#7215 = DIRECTION ( 'NONE',  ( -1.000000000000000000, -0.000000000000000000, -0.000000000000000000 ) ) ;
#7216 = CARTESIAN_POINT ( 'NONE',  ( -823.1581254408797577, 73.70809864670201250, -142.8810402703304021 ) ) ;
#7217 = DIRECTION ( 'NONE',  ( 0.000000000000000000, 0.000000000000000000, -1.000000000000000000 ) ) ;
#7218 = CARTESIAN_POINT ( 'NONE',  ( -144.0488662551579182, 12.00000000000000000, -146.9077238332691877 ) ) ;
#7219 = CARTESIAN_POINT ( 'NONE',  ( -819.3349937000580212, 76.45728329316879979, -154.6806410948596806 ) ) ;
#7220 = AXIS2_PLACEMENT_3D ( 'NONE', #6332, #4426, #8203 ) ;
#7221 = VERTEX_POINT ( 'NONE', #2999 ) ;
#7222 = DIRECTION ( 'NONE',  ( 0.000000000000000000, 0.000000000000000000, 1.000000000000000000 ) ) ;
#7223 = CARTESIAN_POINT ( 'NONE',  ( -1045.884592419585942, 115.0579440276405450, -118.7903414690682524 ) ) ;
#7224 = FACE_OUTER_BOUND ( 'NONE', #10021, .T. ) ;
#7225 = CARTESIAN_POINT ( 'NONE',  ( 0.000000000000000000, 81.99999999999995737, -159.6807709998038547 ) ) ;
#7226 = CARTESIAN_POINT ( 'NONE',  ( 1.387778780781445676E-14, -58.00000000000000711, 133.9213562373095101 ) ) ;
#7227 = CARTESIAN_POINT ( 'NONE',  ( 19.96063188563586266, 182.4486063944580678, -125.9423908938470333 ) ) ;
#7228 = EDGE_CURVE ( 'NONE', #2921, #4471, #4828, .T. ) ;
#7229 = ORIENTED_EDGE ( 'NONE', *, *, #10550, .T. ) ;
#7230 = EDGE_CURVE ( 'NONE', #8717, #8333, #10362, .T. ) ;
#7231 = VERTEX_POINT ( 'NONE', #2077 ) ;
#7232 = CIRCLE ( 'NONE', #1504, 7.500000000000007105 ) ;
#7233 = CARTESIAN_POINT ( 'NONE',  ( 4.255174644013695128E-15, 25.00000000000002132, -126.4213562373094959 ) ) ;
#7234 = CARTESIAN_POINT ( 'NONE',  ( -385.0037317092140370, 81.69534135820630638, -144.6874058649623862 ) ) ;
#7235 = CARTESIAN_POINT ( 'NONE',  ( -822.4997677527437645, 73.84243176666275588, -142.9416447491881286 ) ) ;
#7236 = DIRECTION ( 'NONE',  ( 0.000000000000000000, 0.000000000000000000, 1.000000000000000000 ) ) ;
#7237 = DIRECTION ( 'NONE',  ( 2.081668171172161734E-17, 4.930380657631307143E-31, -1.000000000000000000 ) ) ;
#7238 = ORIENTED_EDGE ( 'NONE', *, *, #4512, .F. ) ;
#7239 = DIRECTION ( 'NONE',  ( -8.163404592832030268E-17, 1.000000000000000000, -0.000000000000000000 ) ) ;
#7240 = CYLINDRICAL_SURFACE ( 'NONE', #9231, 7.500000000000007105 ) ;
#7241 = VERTEX_POINT ( 'NONE', #4967 ) ;
#7242 = CARTESIAN_POINT ( 'NONE',  ( -30.00000000000000000, -6.000000000000000000, 30.00000000000000000 ) ) ;
#7243 = CARTESIAN_POINT ( 'NONE',  ( -1025.323167507848893, 62.35287014669186334, -146.0307792196450691 ) ) ;
#7244 = AXIS2_PLACEMENT_3D ( 'NONE', #1052, #11362, #11299 ) ;
#7245 = CARTESIAN_POINT ( 'NONE',  ( 19.98514591218119563, 182.6308847568197109, -125.4591452170799641 ) ) ;
#7246 = ORIENTED_EDGE ( 'NONE', *, *, #3053, .F. ) ;
#7247 = VERTEX_POINT ( 'NONE', #2136 ) ;
#7248 = DIRECTION ( 'NONE',  ( -1.186840563529527301E-16, 1.000000000000000000, -0.000000000000000000 ) ) ;
#7249 = EDGE_LOOP ( 'NONE', ( #2704, #7341, #5836, #12194, #9467, #5317 ) ) ;
#7250 = AXIS2_PLACEMENT_3D ( 'NONE', #9366, #6456, #6393 ) ;
#7251 = CARTESIAN_POINT ( 'NONE',  ( -370.2091804001356081, 56.54852862931996071, -132.0405513051967716 ) ) ;
#7252 = CARTESIAN_POINT ( 'NONE',  ( -141.4213562373095101, 0.000000000000000000, 3.644282033693712520E-14 ) ) ;
#7253 = ORIENTED_EDGE ( 'NONE', *, *, #3438, .T. ) ;
#7254 = AXIS2_PLACEMENT_3D ( 'NONE', #6299, #8856, #4387 ) ;
#7255 = CARTESIAN_POINT ( 'NONE',  ( -30.00000000000000000, -492.9999999999998863, 30.00000000000000000 ) ) ;
#7256 = EDGE_LOOP ( 'NONE', ( #9084, #11649, #11607, #7853 ) ) ;
#7257 = DIRECTION ( 'NONE',  ( 0.000000000000000000, 0.000000000000000000, 1.000000000000000000 ) ) ;
#7258 = DIRECTION ( 'NONE',  ( 0.000000000000000000, 0.000000000000000000, 1.000000000000000000 ) ) ;
#7259 = DIRECTION ( 'NONE',  ( -0.000000000000000000, -1.000000000000000000, -0.000000000000000000 ) ) ;
#7260 = DIRECTION ( 'NONE',  ( 0.000000000000000000, 0.000000000000000000, 1.000000000000000000 ) ) ;
#7261 = CARTESIAN_POINT ( 'NONE',  ( -305.0000000000000568, 24.00000000000000711, -159.6807709998038547 ) ) ;
#7262 = EDGE_CURVE ( 'NONE', #4792, #3812, #474, .T. ) ;
#7263 = ORIENTED_EDGE ( 'NONE', *, *, #12020, .F. ) ;
#7264 = CIRCLE ( 'NONE', #1942, 7.500000000000007105 ) ;
#7265 = CARTESIAN_POINT ( 'NONE',  ( -21.06224515417718379, 178.9392833470433004, -125.7311303738450050 ) ) ;
#7266 = SHAPE_REPRESENTATION_RELATIONSHIP ( 'NONE' , 'NONE' ,  #690, #8261 ) ;
#7267 = CARTESIAN_POINT ( 'NONE',  ( 35.00000000000000000, 81.99999999999998579, -124.6807709998039826 ) ) ;
#7268 = ORIENTED_EDGE ( 'NONE', *, *, #724, .F. ) ;
#7269 = CARTESIAN_POINT ( 'NONE',  ( -1024.256845364730452, 79.46673622094698430, -95.06748246948041015 ) ) ;
#7270 = FACE_OUTER_BOUND ( 'NONE', #3691, .T. ) ;
#7271 = FACE_OUTER_BOUND ( 'NONE', #5574, .T. ) ;
#7272 = CARTESIAN_POINT ( 'NONE',  ( 20.72444876762976307, 180.4743292376399779, -123.3248083624227291 ) ) ;
#7273 = AXIS2_PLACEMENT_3D ( 'NONE', #1099, #9553, #5721 ) ;
#7274 = CIRCLE ( 'NONE', #4321, 7.500000000000007105 ) ;
#7275 = DIRECTION ( 'NONE',  ( 0.000000000000000000, -1.156482317317870246E-16, 1.000000000000000000 ) ) ;
#7276 = CARTESIAN_POINT ( 'NONE',  ( -19.96345380219486643, 178.1547366163775905, -123.4647820529329323 ) ) ;
#7277 = DIRECTION ( 'NONE',  ( 0.000000000000000000, -1.000000000000000000, -7.930164461608263644E-17 ) ) ;
#7278 = EDGE_CURVE ( 'NONE', #8433, #69, #7755, .T. ) ;
#7279 = ORIENTED_EDGE ( 'NONE', *, *, #10327, .F. ) ;
#7280 = DIRECTION ( 'NONE',  ( 0.000000000000000000, 1.000000000000000000, 0.000000000000000000 ) ) ;
#7281 = CARTESIAN_POINT ( 'NONE',  ( -819.0908945849121210, 77.06763757931493330, -154.6734934370493306 ) ) ;
#7282 = ADVANCED_FACE ( 'NONE', ( #11528 ), #5899, .F. ) ;
#7283 = AXIS2_PLACEMENT_3D ( 'NONE', #12053, #6613, #2784 ) ;
#7284 = VERTEX_POINT ( 'NONE', #2193 ) ;
#7285 = DIRECTION ( 'NONE',  ( -4.236366511936864528E-16, 1.000000000000000000, 5.522905491341393153E-16 ) ) ;
#7286 = CARTESIAN_POINT ( 'NONE',  ( -1013.901471336336158, 119.8325901201402814, -118.7903414690677835 ) ) ;
#7287 = CARTESIAN_POINT ( 'NONE',  ( 0.000000000000000000, -58.00000000000000711, -126.4213562373094959 ) ) ;
#7288 = DIRECTION ( 'NONE',  ( 0.000000000000000000, 0.000000000000000000, -1.000000000000000000 ) ) ;
#7289 = CARTESIAN_POINT ( 'NONE',  ( -90.00000000000000000, 152.0000000000000000, -126.4213562373088564 ) ) ;
#7290 = EDGE_CURVE ( 'NONE', #2055, #4489, #5821, .T. ) ;
#7291 = CARTESIAN_POINT ( 'NONE',  ( 19.91016817870376343, 181.9717396535510261, -126.5779665355682084 ) ) ;
#7292 = VERTEX_POINT ( 'NONE', #8860 ) ;
#7293 = CIRCLE ( 'NONE', #4328, 7.500000000000007105 ) ;
#7294 = VECTOR ( 'NONE', #11792, 1000.000000000000000 ) ;
#7295 = ORIENTED_EDGE ( 'NONE', *, *, #9725, .F. ) ;
#7296 = CARTESIAN_POINT ( 'NONE',  ( -1017.810720698609543, 119.7719591276204625, -124.6807709998040679 ) ) ;
#7297 = CARTESIAN_POINT ( 'NONE',  ( -19.83159839258490820, 180.4039558769570704, -127.2706957209718581 ) ) ;
#7298 = DIRECTION ( 'NONE',  ( 0.000000000000000000, 1.000000000000000000, 0.000000000000000000 ) ) ;
#7299 = CARTESIAN_POINT ( 'NONE',  ( -927.1204550305436669, 105.3607176047074745, -152.5758913445291114 ) ) ;
#7300 = CARTESIAN_POINT ( 'NONE',  ( -372.6517233435575918, 101.1862970994316697, -130.5563829983385347 ) ) ;
#7301 = DIRECTION ( 'NONE',  ( 0.000000000000000000, 1.000000000000000000, 0.000000000000000000 ) ) ;
#7302 = CARTESIAN_POINT ( 'NONE',  ( 6.899999999999999467, 5.196152422706624918, 8.999999999999998224 ) ) ;
#7303 = CARTESIAN_POINT ( 'NONE',  ( -927.1204550305436669, 105.3607176047074745, -152.5758913445291114 ) ) ;
#7304 = PLANE ( 'NONE',  #4241 ) ;
#7305 = ORIENTED_EDGE ( 'NONE', *, *, #6298, .F. ) ;
#7306 = PLANE ( 'NONE',  #160 ) ;
#7308 = EDGE_CURVE ( 'NONE', #9092, #4723, #6558, .T. ) ;
#7307 = DIRECTION ( 'NONE',  ( -0.05071605604150816737, 0.8431788344085415776, -0.5352357750235388067 ) ) ;
#7309 = ORIENTED_EDGE ( 'NONE', *, *, #1083, .T. ) ;
#7310 = CARTESIAN_POINT ( 'NONE',  ( 9.371890508914830252E-13, 152.0000000000000000, -28.92135623730947458 ) ) ;
#7311 = CARTESIAN_POINT ( 'NONE',  ( -1032.113539130925574, 67.34854938887519893, -152.5758913445294240 ) ) ;
#7312 = ORIENTED_EDGE ( 'NONE', *, *, #3978, .T. ) ;
#7313 = ADVANCED_FACE ( 'NONE', ( #1864 ), #3514, .F. ) ;
#7314 = LINE ( 'NONE', #12073, #3439 ) ;
#7315 = CARTESIAN_POINT ( 'NONE',  ( -21.06351426534828519, 179.8693486757446465, -126.3917480513811711 ) ) ;
#7316 = VERTEX_POINT ( 'NONE', #10206 ) ;
#7317 = CARTESIAN_POINT ( 'NONE',  ( -369.9778043404595564, 55.96332071781321105, -128.6253823055326961 ) ) ;
#7318 = DIRECTION ( 'NONE',  ( 0.000000000000000000, 1.000000000000000000, 0.000000000000000000 ) ) ;
#7319 = VERTEX_POINT ( 'NONE', #9281 ) ;
#7320 = ADVANCED_FACE ( 'NONE', ( #9461 ), #819, .F. ) ;
#7321 = ORIENTED_EDGE ( 'NONE', *, *, #9393, .F. ) ;
#7322 = DIRECTION ( 'NONE',  ( 0.9501779778103313090, 0.000000000000000000, -0.3117078928809301486 ) ) ;
#7323 = LINE ( 'NONE', #1255, #4653 ) ;
#7324 = CARTESIAN_POINT ( 'NONE',  ( 3.123963502971610252E-13, 0.000000000000000000, -96.42135623730949590 ) ) ;
#7325 = CARTESIAN_POINT ( 'NONE',  ( 19.98090249381007766, 179.4171559229623654, -125.9448273171951627 ) ) ;
#7326 = CARTESIAN_POINT ( 'NONE',  ( -952.6992609796628813, 94.45070821374962122, -95.06748246947989855 ) ) ;
#7327 = DIRECTION ( 'NONE',  ( 1.000000000000000000, 0.000000000000000000, -0.000000000000000000 ) ) ;
#7328 = DIRECTION ( 'NONE',  ( 2.040851148208007875E-17, -1.000000000000000000, -0.000000000000000000 ) ) ;
#7329 = CARTESIAN_POINT ( 'NONE',  ( -374.0809930161825605, 70.68769334614165700, -97.60498186712243296 ) ) ;
#7330 = ORIENTED_EDGE ( 'NONE', *, *, #9624, .T. ) ;
#7331 = CARTESIAN_POINT ( 'NONE',  ( -823.1761409384598664, 83.64233031452180001, -144.6133277457489612 ) ) ;
#7332 = EDGE_LOOP ( 'NONE', ( #6904, #8815, #6818, #58 ) ) ;
#7333 = DIRECTION ( 'NONE',  ( -1.000000000000000000, 0.000000000000000000, 0.000000000000000000 ) ) ;
#7334 = CARTESIAN_POINT ( 'NONE',  ( 144.0488662551573782, 12.00000000000000000, -139.4077238332702109 ) ) ;
#7335 = DIRECTION ( 'NONE',  ( 0.000000000000000000, 0.000000000000000000, 1.000000000000000000 ) ) ;
#7336 = LINE ( 'NONE', #6472, #10057 ) ;
#7337 = CARTESIAN_POINT ( 'NONE',  ( -20.80350290787439960, 179.2386340239274887, -123.6703652008354055 ) ) ;
#7338 = CARTESIAN_POINT ( 'NONE',  ( -827.8145948178535036, 75.63860347950554797, -143.6442145102265329 ) ) ;
#7339 = VECTOR ( 'NONE', #11791, 1000.000000000000000 ) ;
#7340 = VERTEX_POINT ( 'NONE', #3092 ) ;
#7341 = ORIENTED_EDGE ( 'NONE', *, *, #10937, .T. ) ;
#7342 = CARTESIAN_POINT ( 'NONE',  ( -370.7999735434212880, 58.11281947991218999, -137.1733638493476519 ) ) ;
#7343 = CONTEXT_DEPENDENT_SHAPE_REPRESENTATION ( #9454, #4086 ) ;
#7344 = EDGE_LOOP ( 'NONE', ( #1980, #2708, #984, #1096 ) ) ;
#7345 = CARTESIAN_POINT ( 'NONE',  ( -1060.846413679908210, 110.5345601522217720, -113.1262384684099374 ) ) ;
#7346 = CARTESIAN_POINT ( 'NONE',  ( -30.00000000000000000, 152.0000000000000000, -126.4213562373092685 ) ) ;
#7347 = LINE ( 'NONE', #6352, #8470 ) ;
#7348 = CARTESIAN_POINT ( 'NONE',  ( -373.0722496536144490, 65.67588619885601986, -101.1744612802395125 ) ) ;
#7349 = AXIS2_PLACEMENT_3D ( 'NONE', #2973, #6623, #1928 ) ;
#7350 = ADVANCED_FACE ( 'NONE', ( #9699 ), #12025, .F. ) ;
#7351 = CARTESIAN_POINT ( 'NONE',  ( 19.99873220238463389, 182.6645275560894106, -124.4081891067125838 ) ) ;
#7352 = EDGE_CURVE ( 'NONE', #10844, #4515, #10952, .T. ) ;
#7353 = VERTEX_POINT ( 'NONE', #12096 ) ;
#7354 = ORIENTED_EDGE ( 'NONE', *, *, #6298, .T. ) ;
#7355 = CYLINDRICAL_SURFACE ( 'NONE', #7091, 20.00000000000004619 ) ;
#7356 = CARTESIAN_POINT ( 'NONE',  ( 35.00000000000000000, 81.99999999999998579, 272.3192290001959464 ) ) ;
#7357 = CARTESIAN_POINT ( 'NONE',  ( -1023.078931369431530, 98.73915068298377662, -152.5758913445292535 ) ) ;
#7358 = CARTESIAN_POINT ( 'NONE',  ( -369.9085427289805921, 108.2084335843136387, -126.6389740589983433 ) ) ;
#7359 = EDGE_CURVE ( 'NONE', #4907, #7819, #3481, .T. ) ;
#7360 = FILL_AREA_STYLE_COLOUR ( '', #3139 ) ;
#7361 = CARTESIAN_POINT ( 'NONE',  ( 0.01899995639453445906, 7.352259170992713422, -5.265513565426380715 ) ) ;
#7362 = CARTESIAN_POINT ( 'NONE',  ( -853.2189900670995257, 91.12674563889149226, -152.5758913445289693 ) ) ;
#7363 = ORIENTED_EDGE ( 'NONE', *, *, #2285, .T. ) ;
#7364 = DIRECTION ( 'NONE',  ( 0.000000000000000000, 0.000000000000000000, 1.000000000000000000 ) ) ;
#7365 = DIRECTION ( 'NONE',  ( -1.000000000000000000, 0.000000000000000000, 0.000000000000000000 ) ) ;
#7366 = EDGE_LOOP ( 'NONE', ( #6545, #6320, #10956, #55 ) ) ;
#7367 = CARTESIAN_POINT ( 'NONE',  ( -819.2376510598713821, 55.50059629688480811, -152.5758913445292535 ) ) ;
#7368 = CARTESIAN_POINT ( 'NONE',  ( -20.77482174596494247, 180.9926187296578348, -123.5402880645763730 ) ) ;
#7369 = ORIENTED_EDGE ( 'NONE', *, *, #1201, .T. ) ;
#7370 = VERTEX_POINT ( 'NONE', #1707 ) ;
#7371 = EDGE_CURVE ( 'NONE', #2076, #4751, #287, .T. ) ;
#7372 = CARTESIAN_POINT ( 'NONE',  ( -21.06676927307846725, 179.4988070236175588, -126.2505506485803153 ) ) ;
#7373 = CARTESIAN_POINT ( 'NONE',  ( 1.387778780781445676E-14, -6.000000000000000000, 126.4213562373094959 ) ) ;
#7374 = AXIS2_PLACEMENT_3D ( 'NONE', #6414, #799, #10056 ) ;
#7375 = VERTEX_POINT ( 'NONE', #9243 ) ;
#7376 = ADVANCED_FACE ( 'NONE', ( #359 ), #2283, .F. ) ;
#7377 = CARTESIAN_POINT ( 'NONE',  ( -373.1538797604212050, 64.77014134620993957, -134.9108730226440969 ) ) ;
#7378 = CARTESIAN_POINT ( 'NONE',  ( -818.8285638327251945, 78.67432280806566780, -154.6235849673217899 ) ) ;
#7379 = CARTESIAN_POINT ( 'NONE',  ( -232.4999999999999716, 12.00000000000001066, -126.4213562373078190 ) ) ;
#7380 = EDGE_LOOP ( 'NONE', ( #8495, #1727, #7424, #886 ) ) ;
#7381 = CARTESIAN_POINT ( 'NONE',  ( 13.32222501832753991, 180.2041921146325762, -184.1652315311844177 ) ) ;
#7382 = AXIS2_PLACEMENT_3D ( 'NONE', #4757, #8532, #1234 ) ;
#7383 = CARTESIAN_POINT ( 'NONE',  ( 0.1469846612282405540, -6.696526368584445166, 6.401276095386996268 ) ) ;
#7384 = DIRECTION ( 'NONE',  ( -8.163404592832030268E-17, 1.000000000000000000, -0.000000000000000000 ) ) ;
#7385 = CARTESIAN_POINT ( 'NONE',  ( -819.3361059452977315, 80.89324539545522441, -154.4704897894791031 ) ) ;
#7386 = EDGE_CURVE ( 'NONE', #10168, #8630, #7314, .T. ) ;
#7387 = CARTESIAN_POINT ( 'NONE',  ( -1056.743458481016432, 64.45745743522633120, -96.78565065507969223 ) ) ;
#7388 = DIRECTION ( 'NONE',  ( 0.000000000000000000, 0.000000000000000000, 1.000000000000000000 ) ) ;
#7389 = DIRECTION ( 'NONE',  ( -1.000000000000000000, -0.000000000000000000, -0.000000000000000000 ) ) ;
#7390 = ORIENTED_EDGE ( 'NONE', *, *, #8880, .T. ) ;
#7391 = CIRCLE ( 'NONE', #891, 7.500000000000007105 ) ;
#7392 = CARTESIAN_POINT ( 'NONE',  ( -823.5011194091124480, 83.67446401253047839, -144.6105519893419000 ) ) ;
#7393 = TOROIDAL_SURFACE ( 'NONE', #2066, 8.500000000000003553, 1.000000000000000000 ) ;
#7394 = CIRCLE ( 'NONE', #11343, 7.500000000000007105 ) ;
#7395 = CARTESIAN_POINT ( 'NONE',  ( -369.8899886004867881, 108.2543221321664930, -124.8540024292112065 ) ) ;
#7396 = ORIENTED_EDGE ( 'NONE', *, *, #5479, .T. ) ;
#7397 = DIRECTION ( 'NONE',  ( -2.081668171172161734E-17, -4.930380657631307143E-31, 1.000000000000000000 ) ) ;
#7398 = CARTESIAN_POINT ( 'NONE',  ( -975.9242088207895449, 48.36955882740807766, -103.3307627799632513 ) ) ;
#7399 = DIRECTION ( 'NONE',  ( 0.000000000000000000, 0.000000000000000000, 1.000000000000000000 ) ) ;
#7400 = DIRECTION ( 'NONE',  ( -1.186840563529527301E-16, 1.000000000000000000, 0.000000000000000000 ) ) ;
#7401 = DIRECTION ( 'NONE',  ( 0.000000000000000000, 0.000000000000000000, 1.000000000000000000 ) ) ;
#7402 = AXIS2_PLACEMENT_3D ( 'NONE', #881, #4654, #2913 ) ;
#7403 = CARTESIAN_POINT ( 'NONE',  ( 4.808665244885994618E-14, -6.000000000000000000, 141.4213562373094817 ) ) ;
#7404 = CARTESIAN_POINT ( 'NONE',  ( -20.81794809838210369, 179.1660952925545871, -123.7384776798486143 ) ) ;
#7405 = CARTESIAN_POINT ( 'NONE',  ( -827.1548796934557686, 74.92718183615713201, -143.3900093790822439 ) ) ;
#7406 = ORIENTED_EDGE ( 'NONE', *, *, #6901, .T. ) ;
#7407 = ORIENTED_EDGE ( 'NONE', *, *, #7508, .F. ) ;
#7408 = CARTESIAN_POINT ( 'NONE',  ( -369.9667548185103669, 55.93616024285574895, -121.0690321629715669 ) ) ;
#7409 = ORIENTED_EDGE ( 'NONE', *, *, #6770, .T. ) ;
#7410 = CARTESIAN_POINT ( 'NONE',  ( -1061.104375862967800, 103.3839434440458547, -103.3307627799635924 ) ) ;
#7411 = AXIS2_PLACEMENT_3D ( 'NONE', #6106, #11222, #10095 ) ;
#7412 = CARTESIAN_POINT ( 'NONE',  ( 21.06778026255562253, 181.0036129245391976, -126.2017578805543820 ) ) ;
#7413 = DIRECTION ( 'NONE',  ( 2.040851148208007875E-17, -1.000000000000000000, -0.000000000000000000 ) ) ;
#7414 = CARTESIAN_POINT ( 'NONE',  ( -371.0944895696485446, 58.94320524275045159, -110.3215891064999994 ) ) ;
#7415 = CARTESIAN_POINT ( 'NONE',  ( 20.93432090161336490, 181.6310399508034834, -124.3821073715919852 ) ) ;
#7416 = ORIENTED_EDGE ( 'NONE', *, *, #9158, .F. ) ;
#7417 = EDGE_LOOP ( 'NONE', ( #6202, #11645 ) ) ;
#7418 = CARTESIAN_POINT ( 'NONE',  ( -1021.743962174751232, 119.2557508373789403, -124.6807709998040110 ) ) ;
#7419 = CYLINDRICAL_SURFACE ( 'NONE', #7549, 7.500000000000007105 ) ;
#7420 = DIRECTION ( 'NONE',  ( 0.000000000000000000, -0.5000000000000018874, -0.8660254037844375974 ) ) ;
#7421 = CARTESIAN_POINT ( 'NONE',  ( -1011.935294340112478, 99.50314415908300703, -152.5758913445291967 ) ) ;
#7422 = ADVANCED_FACE ( 'NONE', ( #11077, #8114 ), #180, .T. ) ;
#7423 = CYLINDRICAL_SURFACE ( 'NONE', #1476, 5.000000000000115463 ) ;
#7424 = ORIENTED_EDGE ( 'NONE', *, *, #4885, .T. ) ;
#7425 = CARTESIAN_POINT ( 'NONE',  ( -262.5000000000000000, -9.213203435596478030, -126.4213562373076059 ) ) ;
#7426 = ORIENTED_EDGE ( 'NONE', *, *, #5723, .T. ) ;
#7427 = CARTESIAN_POINT ( 'NONE',  ( -1056.106496161729183, 78.18408418063155807, -154.8742214401234776 ) ) ;
#7428 = CARTESIAN_POINT ( 'NONE',  ( 19.88629874799092789, 181.6918713317650713, -126.8133243770599421 ) ) ;
#7429 = ORIENTED_EDGE ( 'NONE', *, *, #4516, .T. ) ;
#7430 = CIRCLE ( 'NONE', #8439, 1.000000000000000888 ) ;
#7431 = ORIENTED_EDGE ( 'NONE', *, *, #1187, .T. ) ;
#7432 = ORIENTED_EDGE ( 'NONE', *, *, #6903, .T. ) ;
#7433 = CARTESIAN_POINT ( 'NONE',  ( -374.1032283779920817, 69.49316288506409478, -140.3724387714157444 ) ) ;
#7434 = DIRECTION ( 'NONE',  ( -1.000000000000000000, 0.000000000000000000, 0.000000000000000000 ) ) ;
#7435 = EDGE_CURVE ( 'NONE', #11584, #2214, #1008, .T. ) ;
#7436 = AXIS2_PLACEMENT_3D ( 'NONE', #1888, #9102, #7333 ) ;
#7437 = CARTESIAN_POINT ( 'NONE',  ( 9.371890508914830252E-13, -6.000000000000005329, -36.42135623730949590 ) ) ;
#7438 = ORIENTED_EDGE ( 'NONE', *, *, #3726, .T. ) ;
#7439 = DIRECTION ( 'NONE',  ( 1.000000000000000000, 0.000000000000000000, 0.000000000000000000 ) ) ;
#7440 = EDGE_CURVE ( 'NONE', #9588, #8369, #3, .T. ) ;
#7441 = CARTESIAN_POINT ( 'NONE',  ( 9.184850993605159777E-16, -58.00000000000000711, -133.9213562373095101 ) ) ;
#7442 = CARTESIAN_POINT ( 'NONE',  ( 6.899999999999999467, -5.196152422706606266, 8.999999999999998224 ) ) ;
#7443 = CIRCLE ( 'NONE', #5260, 7.499999999999992895 ) ;
#7444 = CARTESIAN_POINT ( 'NONE',  ( -795.0000000000022737, 65.22545431197607968, -99.57582448894522997 ) ) ;
#7445 = CARTESIAN_POINT ( 'NONE',  ( 6.899999999999999467, 7.794228634059940042, -4.500000000000007105 ) ) ;
#7446 = CARTESIAN_POINT ( 'NONE',  ( -379.1619848709565304, 102.0000000000000142, -125.7938822953540381 ) ) ;
#7447 = ORIENTED_EDGE ( 'NONE', *, *, #5034, .T. ) ;
#7448 = CARTESIAN_POINT ( 'NONE',  ( -818.9871366297743407, 79.96561131120978416, -144.5796535119514488 ) ) ;
#7449 = DIRECTION ( 'NONE',  ( 1.000000000000000000, 0.000000000000000000, 0.000000000000000000 ) ) ;
#7450 = FILL_AREA_STYLE_COLOUR ( '', #2880 ) ;
#7451 = EDGE_CURVE ( 'NONE', #12119, #4907, #11352, .T. ) ;
#7452 = ORIENTED_EDGE ( 'NONE', *, *, #5111, .T. ) ;
#7453 = TOROIDAL_SURFACE ( 'NONE', #8228, 44.00000000000000711, 1.000000000000000000 ) ;
#7454 = EDGE_CURVE ( 'NONE', #10844, #1640, #6739, .T. ) ;
#7455 = CARTESIAN_POINT ( 'NONE',  ( -1025.323167507843664, 62.35287014669171413, -103.3307627799636350 ) ) ;
#7456 = AXIS2_PLACEMENT_3D ( 'NONE', #1621, #763, #10955 ) ;
#7457 = EDGE_CURVE ( 'NONE', #2455, #9741, #5623, .T. ) ;
#7458 = DIRECTION ( 'NONE',  ( -1.000000000000000000, -4.236366511936864528E-16, -3.037002292462560327E-31 ) ) ;
#7459 = DIRECTION ( 'NONE',  ( 0.000000000000000000, 1.000000000000000000, 0.000000000000000000 ) ) ;
#7460 = CARTESIAN_POINT ( 'NONE',  ( -210.0000000000000000, 151.9999999999999716, -126.4213562373080180 ) ) ;
#7461 = CARTESIAN_POINT ( 'NONE',  ( 0.000000000000000000, 152.0000000000000000, -124.6807709998038405 ) ) ;
#7462 = EDGE_CURVE ( 'NONE', #759, #9388, #10517, .T. ) ;
#7463 = EDGE_CURVE ( 'NONE', #3418, #3398, #4053, .T. ) ;
#7464 = CARTESIAN_POINT ( 'NONE',  ( -819.0854767918228845, 77.05939038872129743, -105.2981374327913358 ) ) ;
#7465 = CARTESIAN_POINT ( 'NONE',  ( -20.94242073755689404, 178.7541906832940128, -124.4271745170988055 ) ) ;
#7466 = CARTESIAN_POINT ( 'NONE',  ( -821.2963138009649811, 74.35985007445651718, -143.1641509997125183 ) ) ;
#7467 = VECTOR ( 'NONE', #6748, 1000.000000000000000 ) ;
#7468 = ORIENTED_EDGE ( 'NONE', *, *, #6937, .F. ) ;
#7469 = CARTESIAN_POINT ( 'NONE',  ( -373.9059702089900270, 69.66321476674123403, -151.1683612898431477 ) ) ;
#7470 = CARTESIAN_POINT ( 'NONE',  ( -374.4452484659049105, 92.10134583476683190, -107.3453501722017052 ) ) ;
#7471 = VERTEX_POINT ( 'NONE', #1134 ) ;
#7472 = CARTESIAN_POINT ( 'NONE',  ( -1054.913455627178109, 103.6024512377076263, -103.3307627799635640 ) ) ;
#7473 = EDGE_CURVE ( 'NONE', #8380, #3503, #3058, .T. ) ;
#7474 = CIRCLE ( 'NONE', #11810, 1.000000000000000000 ) ;
#7475 = CIRCLE ( 'NONE', #8662, 0.9999999999999905631 ) ;
#7476 = CARTESIAN_POINT ( 'NONE',  ( 20.82544450079020848, 181.2865457812275736, -123.7704112417842879 ) ) ;
#7477 = ORIENTED_EDGE ( 'NONE', *, *, #4033, .F. ) ;
#7478 = VERTEX_POINT ( 'NONE', #10459 ) ;
#7479 = TOROIDAL_SURFACE ( 'NONE', #9849, 14.02076803445813269, 1.499999999999998002 ) ;
#7480 = LINE ( 'NONE', #11369, #787 ) ;
#7481 = DIRECTION ( 'NONE',  ( 1.000000000000000000, 0.000000000000000000, 0.000000000000000000 ) ) ;
#7482 = CARTESIAN_POINT ( 'NONE',  ( -975.1903095749692056, 79.73237568579439483, -154.8742214401228523 ) ) ;
#7483 = CARTESIAN_POINT ( 'NONE',  ( -379.6804543574866670, 101.1236513765119724, -118.8160366733158639 ) ) ;
#7484 = AXIS2_PLACEMENT_3D ( 'NONE', #6781, #10497, #4129 ) ;
#7485 = DIRECTION ( 'NONE',  ( 1.000000000000000000, 0.000000000000000000, 0.000000000000000000 ) ) ;
#7486 = CARTESIAN_POINT ( 'NONE',  ( 0.000000000000000000, 0.000000000000000000, -126.4213562373094959 ) ) ;
#7487 =( NAMED_UNIT ( * ) SI_UNIT ( $, .STERADIAN. ) SOLID_ANGLE_UNIT ( ) );
#7488 = ORIENTED_EDGE ( 'NONE', *, *, #8441, .F. ) ;
#7489 = LINE ( 'NONE', #1675, #12227 ) ;
#7490 = CARTESIAN_POINT ( 'NONE',  ( -374.5977935108010684, 90.76354315037471565, -142.7312558896330756 ) ) ;
#7491 = EDGE_LOOP ( 'NONE', ( #7305, #10789, #12082, #9620 ) ) ;
#7492 = CARTESIAN_POINT ( 'NONE',  ( -1031.794838716557251, 81.34535957697963227, -154.8742214401231649 ) ) ;
#7493 = STYLED_ITEM ( 'NONE', ( #3638 ), #3860 ) ;
#7494 = EDGE_LOOP ( 'NONE', ( #9053, #11774, #6774, #4293 ) ) ;
#7495 = ORIENTED_EDGE ( 'NONE', *, *, #6003, .F. ) ;
#7496 = CARTESIAN_POINT ( 'NONE',  ( -828.6712641482290564, 79.96111424986135319, -144.5792126457448603 ) ) ;
#7497 = CARTESIAN_POINT ( 'NONE',  ( -826.0807747705229076, 74.19805998537532332, -106.2647609865424556 ) ) ;
#7498 = VERTEX_POINT ( 'NONE', #6803 ) ;
#7499 = CARTESIAN_POINT ( 'NONE',  ( -382.3282078984223631, 68.32957519679821701, -139.2830325097624495 ) ) ;
#7500 = CARTESIAN_POINT ( 'NONE',  ( 6.899999999999999467, 8.999999999999998224, 0.000000000000000000 ) ) ;
#7501 = CIRCLE ( 'NONE', #4339, 7.500000000000007105 ) ;
#7502 = B_SPLINE_CURVE_WITH_KNOTS ( 'NONE', 3,
 ( #11738, #3252, #4190, #7029, #11621, #2452, #10919, #5171, #7966, #9812 ),
 .UNSPECIFIED., .F., .F.,
 ( 4, 2, 2, 2, 4 ),
 ( 0.005592014383449837173, 0.006175065507308098722, 0.006758116631166361139, 0.007341167755024623556, 0.007924218878882885106 ),
 .UNSPECIFIED. ) ;
#7503 = DIRECTION ( 'NONE',  ( 0.000000000000000000, -1.156482317317870246E-16, 1.000000000000000000 ) ) ;
#7504 = VERTEX_POINT ( 'NONE', #2922 ) ;
#7505 = EDGE_CURVE ( 'NONE', #5900, #9223, #1072, .T. ) ;
#7506 = DIRECTION ( 'NONE',  ( 0.000000000000000000, 0.000000000000000000, -1.000000000000000000 ) ) ;
#7507 = LINE ( 'NONE', #841, #4024 ) ;
#7508 = EDGE_CURVE ( 'NONE', #2620, #7353, #6615, .T. ) ;
#7509 = CARTESIAN_POINT ( 'NONE',  ( -1057.521967982379238, 48.25222617154000204, -107.9061927053324723 ) ) ;
#7510 = CARTESIAN_POINT ( 'NONE',  ( -818.8285638327240576, 78.67432280806558254, -104.9592124606052295 ) ) ;
#7511 = DIRECTION ( 'NONE',  ( -0.000000000000000000, 1.000000000000000000, 0.000000000000000000 ) ) ;
#7512 = CARTESIAN_POINT ( 'NONE',  ( -795.0000000000036380, 52.00000000000027711, -126.6442663926292624 ) ) ;
#7513 = EDGE_LOOP ( 'NONE', ( #5719, #1903, #4682, #889 ) ) ;
#7514 = CARTESIAN_POINT ( 'NONE',  ( 0.000000000000000000, -485.4999999999998863, -126.4213562373094959 ) ) ;
#7515 = DIRECTION ( 'NONE',  ( 0.000000000000000000, 0.000000000000000000, 1.000000000000000000 ) ) ;
#7516 = EDGE_LOOP ( 'NONE', ( #573, #1381, #780, #2100, #765 ) ) ;
#7517 = DIRECTION ( 'NONE',  ( -0.000000000000000000, 1.000000000000000000, 7.930164461608263644E-17 ) ) ;
#7518 = CARTESIAN_POINT ( 'NONE',  ( -1028.259718048105469, 56.21337363619640115, -107.9061927053325434 ) ) ;
#7519 = FACE_OUTER_BOUND ( 'NONE', #12026, .T. ) ;
#7520 = DIRECTION ( 'NONE',  ( 0.000000000000000000, 0.000000000000000000, 1.000000000000000000 ) ) ;
#7521 = CARTESIAN_POINT ( 'NONE',  ( -823.8285638327243987, 78.67432280806571043, -264.6807709998050200 ) ) ;
#7522 = CARTESIAN_POINT ( 'NONE',  ( 19.87268743161337170, 178.9255784920988503, -126.9338343023757290 ) ) ;
#7523 = CARTESIAN_POINT ( 'NONE',  ( -825.4664863774313517, 73.94730815836251736, -106.3734765325340561 ) ) ;
#7524 = DIRECTION ( 'NONE',  ( 0.000000000000000000, 1.000000000000000000, 0.000000000000000000 ) ) ;
#7525 = EDGE_CURVE ( 'NONE', #4723, #11269, #5732, .T. ) ;
#7526 = B_SPLINE_CURVE_WITH_KNOTS ( 'NONE', 3,
 ( #4467, #6374, #8311, #12067, #3577, #7368 ),
 .UNSPECIFIED., .F., .F.,
 ( 4, 2, 4 ),
 ( 0.003919203138254567960, 0.004336295509814267618, 0.004753387881373966409 ),
 .UNSPECIFIED. ) ;
#7527 = ORIENTED_EDGE ( 'NONE', *, *, #10928, .T. ) ;
#7528 = CYLINDRICAL_SURFACE ( 'NONE', #7769, 7.500000000000007105 ) ;
#7529 = CARTESIAN_POINT ( 'NONE',  ( -380.9366354222731843, 98.78228965653478610, -113.7968190044388450 ) ) ;
#7530 = ORIENTED_EDGE ( 'NONE', *, *, #11971, .T. ) ;
#7531 = CARTESIAN_POINT ( 'NONE',  ( -951.5459139781289650, 122.3346817490815681, -113.1262384684093263 ) ) ;
#7532 = VECTOR ( 'NONE', #7830, 1000.000000000000000 ) ;
#7533 = CARTESIAN_POINT ( 'NONE',  ( -126.4213562373094959, -494.9999999999998863, 7.500000000000035527 ) ) ;
#7534 = CARTESIAN_POINT ( 'NONE',  ( 0.000000000000000000, 12.00000000000000000, -89.68077099980401101 ) ) ;
#7535 = AXIS2_PLACEMENT_3D ( 'NONE', #3309, #2158, #10614 ) ;
#7536 = CARTESIAN_POINT ( 'NONE',  ( -1060.756016675587944, 112.8516620848305934, -122.7172756069790864 ) ) ;
#7537 = ORIENTED_EDGE ( 'NONE', *, *, #7123, .F. ) ;
#7538 = EDGE_CURVE ( 'NONE', #10683, #9067, #5831, .T. ) ;
#7539 = CARTESIAN_POINT ( 'NONE',  ( -59.99999999999998579, -9.213203435596451385, -126.4213562373090696 ) ) ;
#7540 = DIRECTION ( 'NONE',  ( 0.000000000000000000, 0.000000000000000000, 1.000000000000000000 ) ) ;
#7541 = CARTESIAN_POINT ( 'NONE',  ( -795.0000000000080718, 93.55451860843929524, -152.5758913445291398 ) ) ;
#7542 = SURFACE_STYLE_FILL_AREA ( #10379 ) ;
#7543 = CARTESIAN_POINT ( 'NONE',  ( -87.04832655144203102, 12.00000000000000000, -210.4289243767376831 ) ) ;
#7544 = CARTESIAN_POINT ( 'NONE',  ( 8.099999999999999645, 0.000000000000000000, 0.000000000000000000 ) ) ;
#7545 = ORIENTED_EDGE ( 'NONE', *, *, #5371, .F. ) ;
#7546 = VECTOR ( 'NONE', #9823, 1000.000000000000000 ) ;
#7547 = ORIENTED_EDGE ( 'NONE', *, *, #7038, .F. ) ;
#7548 = CARTESIAN_POINT ( 'NONE',  ( -956.2104666674752025, 71.56905446038098262, -152.5758913445294809 ) ) ;
#7549 = AXIS2_PLACEMENT_3D ( 'NONE', #811, #9455, #9272 ) ;
#7550 = FACE_BOUND ( 'NONE', #2436, .T. ) ;
#7551 = ORIENTED_EDGE ( 'NONE', *, *, #9910, .F. ) ;
#7552 = ORIENTED_EDGE ( 'NONE', *, *, #9499, .T. ) ;
#7553 = AXIS2_PLACEMENT_3D ( 'NONE', #7826, #11600, #3871 ) ;
#7554 = DIRECTION ( 'NONE',  ( -0.000000000000000000, -1.000000000000000000, -0.000000000000000000 ) ) ;
#7555 = CARTESIAN_POINT ( 'NONE',  ( -825.4664863774346486, 73.94730815836283000, -106.3734765325343830 ) ) ;
#7556 = ORIENTED_EDGE ( 'NONE', *, *, #4675, .T. ) ;
#7557 = CARTESIAN_POINT ( 'NONE',  ( -384.6392999096204335, 76.78897796811929766, -144.0344280892469158 ) ) ;
#7558 = DIRECTION ( 'NONE',  ( 0.3117078928809249860, -1.670400663243698742E-14, 0.9501779778103330854 ) ) ;
#7559 = CARTESIAN_POINT ( 'NONE',  ( -374.7455030271728447, 74.89167502208620419, -105.9368347594480753 ) ) ;
#7560 = DIRECTION ( 'NONE',  ( 3.061276722312011504E-17, -1.000000000000000000, 0.000000000000000000 ) ) ;
#7561 = ORIENTED_EDGE ( 'NONE', *, *, #10615, .F. ) ;
#7562 = AXIS2_PLACEMENT_3D ( 'NONE', #2182, #4954, #11452 ) ;
#7563 = CARTESIAN_POINT ( 'NONE',  ( -6.106226635438360972E-13, 0.000000000000000000, -244.6807709998039400 ) ) ;
#7564 = CARTESIAN_POINT ( 'NONE',  ( 21.06598783109611261, 179.0588159534046326, -125.8866071576830734 ) ) ;
#7565 = VECTOR ( 'NONE', #8215, 1000.000000000000000 ) ;
#7566 = CARTESIAN_POINT ( 'NONE',  ( -853.7969483066802923, 45.36294356226295577, -99.57582448894520155 ) ) ;
#7567 = CARTESIAN_POINT ( 'NONE',  ( -828.7892213480641885, 79.32116703283894310, -104.8603099499567861 ) ) ;
#7568 = CARTESIAN_POINT ( 'NONE',  ( -1028.581275045468146, 51.02622020309988216, -130.5712005305406080 ) ) ;
#7569 = VERTEX_POINT ( 'NONE', #2190 ) ;
#7570 = FACE_BOUND ( 'NONE', #6816, .T. ) ;
#7571 = EDGE_CURVE ( 'NONE', #1589, #867, #6214, .T. ) ;
#7572 = APPLICATION_PROTOCOL_DEFINITION ( 'draft international standard', 'automotive_design', 1998, #5894 ) ;
#7573 =( NAMED_UNIT ( * ) SI_UNIT ( $, .STERADIAN. ) SOLID_ANGLE_UNIT ( ) );
#7574 = ORIENTED_EDGE ( 'NONE', *, *, #2079, .T. ) ;
#7575 = CARTESIAN_POINT ( 'NONE',  ( -928.2641150402301946, 65.00826535581501275, -107.9061927053325576 ) ) ;
#7576 = FACE_OUTER_BOUND ( 'NONE', #2489, .T. ) ;
#7577 = EDGE_CURVE ( 'NONE', #8293, #8781, #8198, .T. ) ;
#7578 = CARTESIAN_POINT ( 'NONE',  ( 0.8038475772933614261, 5.196152422706624030, -9.000000000000000000 ) ) ;
#7579 = DIRECTION ( 'NONE',  ( 0.000000000000000000, 1.000000000000000000, 2.312964634635740689E-15 ) ) ;
#7580 = DIRECTION ( 'NONE',  ( 0.000000000000000000, 0.000000000000000000, 1.000000000000000000 ) ) ;
#7581 = DIRECTION ( 'NONE',  ( 2.040851148208007875E-17, -1.000000000000000000, -0.000000000000000000 ) ) ;
#7582 = CARTESIAN_POINT ( 'NONE',  ( -19.94693332216800030, 178.0755435337389656, -126.1424034859261525 ) ) ;
#7583 = FACE_OUTER_BOUND ( 'NONE', #8901, .T. ) ;
#7584 = AXIS2_PLACEMENT_3D ( 'NONE', #6474, #796, #8280 ) ;
#7585 = CIRCLE ( 'NONE', #7184, 7.500000000000007105 ) ;
#7586 = VERTEX_POINT ( 'NONE', #9230 ) ;
#7587 = CARTESIAN_POINT ( 'NONE',  ( -823.8285638327245124, 78.67432280806536937, -159.6807709998044800 ) ) ;
#7588 = CARTESIAN_POINT ( 'NONE',  ( -384.4682197693251169, 88.14714501232053578, -105.6460668681738753 ) ) ;
#7589 = VERTEX_POINT ( 'NONE', #9359 ) ;
#7591 = ADVANCED_FACE ( 'NONE', ( #6517 ), #11153, .F. ) ;
#7590 = CARTESIAN_POINT ( 'NONE',  ( -1054.691024341069351, 108.1159421897237110, -107.9061927053325149 ) ) ;
#7592 = FACE_OUTER_BOUND ( 'NONE', #11236, .T. ) ;
#7593 = CARTESIAN_POINT ( 'NONE',  ( -904.0006525278439540, 119.6095687608908378, -141.4553492942759760 ) ) ;
#7594 = DIRECTION ( 'NONE',  ( 0.000000000000000000, 1.000000000000000000, 0.000000000000000000 ) ) ;
#7595 = EDGE_CURVE ( 'NONE', #4244, #10520, #3246, .T. ) ;
#7596 = AXIS2_PLACEMENT_3D ( 'NONE', #4541, #11149, #1919 ) ;
#7597 = CARTESIAN_POINT ( 'NONE',  ( -1017.810720698609543, 119.7719591276204625, -124.6807709998040679 ) ) ;
#7598 = ORIENTED_EDGE ( 'NONE', *, *, #9981, .F. ) ;
#7599 = DIRECTION ( 'NONE',  ( 0.000000000000000000, 1.000000000000000000, 0.000000000000000000 ) ) ;
#7600 = DIRECTION ( 'NONE',  ( 0.000000000000000000, 0.000000000000000000, 1.000000000000000000 ) ) ;
#7601 = DIRECTION ( 'NONE',  ( 0.000000000000000000, 0.000000000000000000, -1.000000000000000000 ) ) ;
#7602 = CARTESIAN_POINT ( 'NONE',  ( -1018.401127491266152, 110.2021201405462136, -146.0307792196445860 ) ) ;
#7603 = CARTESIAN_POINT ( 'NONE',  ( -372.6969993560938406, 101.0120954562736415, -118.4175876187035215 ) ) ;
#7604 = AXIS2_PLACEMENT_3D ( 'NONE', #8387, #1404, #2679 ) ;
#7605 = SURFACE_STYLE_USAGE ( .BOTH. , #10506 ) ;
#7606 = LINE ( 'NONE', #2787, #3047 ) ;
#7607 = AXIS2_PLACEMENT_3D ( 'NONE', #7175, #1548, #5310 ) ;
#7608 = FACE_OUTER_BOUND ( 'NONE', #4196, .T. ) ;
#7609 = ORIENTED_EDGE ( 'NONE', *, *, #2581, .F. ) ;
#7610 = DIRECTION ( 'NONE',  ( -0.000000000000000000, 1.000000000000000000, 7.930164461608263644E-17 ) ) ;
#7611 = CARTESIAN_POINT ( 'NONE',  ( -371.3527037074148325, 104.3051788345223230, -140.5275824910885660 ) ) ;
#7612 = ADVANCED_FACE ( 'NONE', ( #11731 ), #5389, .F. ) ;
#7613 = EDGE_CURVE ( 'NONE', #5102, #6019, #693, .T. ) ;
#7614 = DIRECTION ( 'NONE',  ( -1.000000000000000000, -0.000000000000000000, -0.000000000000000000 ) ) ;
#7615 = EDGE_LOOP ( 'NONE', ( #6356, #2887, #9201, #3740 ) ) ;
#7616 = AXIS2_PLACEMENT_3D ( 'NONE', #6116, #5124, #7852 ) ;
#7617 = ORIENTED_EDGE ( 'NONE', *, *, #3448, .F. ) ;
#7618 = CARTESIAN_POINT ( 'NONE',  ( -20.98070230502330702, 181.7080454659802342, -124.7060752492303095 ) ) ;
#7619 = CARTESIAN_POINT ( 'NONE',  ( -818.8285638327240576, 78.67432280806558254, -104.9592124606052295 ) ) ;
#7620 = CARTESIAN_POINT ( 'NONE',  ( -1016.402231264567945, 68.39482517277122042, -149.7857175106636589 ) ) ;
#7621 = CARTESIAN_POINT ( 'NONE',  ( -374.9952863086498951, 80.93532140996973112, -144.6556666394729120 ) ) ;
#7622 = DIRECTION ( 'NONE',  ( -0.000000000000000000, 1.000000000000000000, -0.000000000000000000 ) ) ;
#7623 = CARTESIAN_POINT ( 'NONE',  ( -384.9453241936137147, 80.00116030919089383, -104.7781441965376814 ) ) ;
#7624 = CARTESIAN_POINT ( 'NONE',  ( -119.9999999999999858, 24.00000000000001421, -126.4213562373086575 ) ) ;
#7625 = AXIS2_PLACEMENT_3D ( 'NONE', #11166, #10292, #11234 ) ;
#7626 = ORIENTED_EDGE ( 'NONE', *, *, #8722, .F. ) ;
#7627 = CARTESIAN_POINT ( 'NONE',  ( -1057.693846703458348, 44.87596864925374973, -136.2353035311986957 ) ) ;
#7628 = VERTEX_POINT ( 'NONE', #3594 ) ;
#7629 = LINE ( 'NONE', #960, #2303 ) ;
#7630 = CARTESIAN_POINT ( 'NONE',  ( -1032.391769651399727, 55.42093464310126905, -103.3307627799637487 ) ) ;
#7631 = DIRECTION ( 'NONE',  ( -1.000000000000000000, -4.236366511936864528E-16, -3.037002292462560327E-31 ) ) ;
#7632 = CARTESIAN_POINT ( 'NONE',  ( -954.5692209181586350, 49.02792041507773746, -122.7172756069790580 ) ) ;
#7633 = ORIENTED_EDGE ( 'NONE', *, *, #1258, .T. ) ;
#7634 = AXIS2_PLACEMENT_3D ( 'NONE', #3554, #8149, #2515 ) ;
#7635 = CARTESIAN_POINT ( 'NONE',  ( -82.49999999999998579, 139.9999999999999716, -126.4213562373088564 ) ) ;
#7636 = ORIENTED_EDGE ( 'NONE', *, *, #5256, .F. ) ;
#7637 = SHAPE_DEFINITION_REPRESENTATION ( #8521, #4872 ) ;
#7638 = LINE ( 'NONE', #2761, #5637 ) ;
#7639 = ORIENTED_EDGE ( 'NONE', *, *, #8739, .F. ) ;
#7640 = CARTESIAN_POINT ( 'NONE',  ( -1048.206790403141440, 45.99070412075073477, -107.9061927053325007 ) ) ;
#7641 = CARTESIAN_POINT ( 'NONE',  ( 1.479627290717497352E-14, 163.9999999999999716, 118.9213562373094817 ) ) ;
#7642 = DIRECTION ( 'NONE',  ( -1.000000000000000000, 0.000000000000000000, 0.000000000000000000 ) ) ;
#7643 = ADVANCED_FACE ( 'NONE', ( #1629 ), #771, .T. ) ;
#7644 = CARTESIAN_POINT ( 'NONE',  ( -1031.086615573502741, 111.8776252365149730, -107.9061927053324723 ) ) ;
#7645 = DIRECTION ( 'NONE',  ( 0.000000000000000000, 0.000000000000000000, 1.000000000000000000 ) ) ;
#7646 = CARTESIAN_POINT ( 'NONE',  ( -21.01574080354420104, 178.7084824148930693, -125.0322960622685144 ) ) ;
#7647 = ORIENTED_EDGE ( 'NONE', *, *, #1558, .F. ) ;
#7648 = CARTESIAN_POINT ( 'NONE',  ( -374.5346922981962052, 90.06812782866809641, -96.12871480239243738 ) ) ;
#7649 = VECTOR ( 'NONE', #2754, 1000.000000000000000 ) ;
#7650 = VERTEX_POINT ( 'NONE', #2554 ) ;
#7651 = CARTESIAN_POINT ( 'NONE',  ( -903.8503739047830550, 115.2915043052427535, -103.3307627799633082 ) ) ;
#7652 = CARTESIAN_POINT ( 'NONE',  ( 0.3570196857253475353, -9.540868182094900618, -1.474731560294319177 ) ) ;
#7653 = CARTESIAN_POINT ( 'NONE',  ( -1010.947924043452645, 120.1731093567702828, -130.5712005305404375 ) ) ;
#7654 = DIRECTION ( 'NONE',  ( -0.000000000000000000, 1.000000000000000000, 0.000000000000000000 ) ) ;
#7655 = ADVANCED_FACE ( 'NONE', ( #8928 ), #11951, .F. ) ;
#7656 = CARTESIAN_POINT ( 'NONE',  ( 7.500000000000008882, 139.9999999999999716, -126.4213562373094959 ) ) ;
#7657 = EDGE_LOOP ( 'NONE', ( #2544, #1974, #7943, #8751 ) ) ;
#7658 = EDGE_CURVE ( 'NONE', #8948, #3787, #2273, .T. ) ;
#7659 = ADVANCED_FACE ( 'NONE', ( #9169 ), #8187, .F. ) ;
#7660 = FACE_OUTER_BOUND ( 'NONE', #9255, .T. ) ;
#7661 = DIRECTION ( 'NONE',  ( 0.000000000000000000, 1.000000000000000000, 0.000000000000000000 ) ) ;
#7662 = CARTESIAN_POINT ( 'NONE',  ( -903.8503739047791896, 115.2915043052427251, -146.0307792196441881 ) ) ;
#7663 = AXIS2_PLACEMENT_3D ( 'NONE', #6591, #1037, #4689 ) ;
#7664 = DIRECTION ( 'NONE',  ( -8.163404592832031500E-17, 1.000000000000000000, 0.000000000000000000 ) ) ;
#7665 = VERTEX_POINT ( 'NONE', #5523 ) ;
#7666 = AXIS2_PLACEMENT_3D ( 'NONE', #11300, #2778, #869 ) ;
#7667 = EDGE_CURVE ( 'NONE', #502, #2477, #11753, .T. ) ;
#7668 = CARTESIAN_POINT ( 'NONE',  ( 19.94988048130710112, 182.0917278327137865, -123.2593186788816695 ) ) ;
#7669 = CARTESIAN_POINT ( 'NONE',  ( -822.7482738817701602, 104.4536172844453148, -146.0307792196443017 ) ) ;
#7670 = FACE_OUTER_BOUND ( 'NONE', #9347, .T. ) ;
#7671 = ORIENTED_EDGE ( 'NONE', *, *, #9780, .F. ) ;
#7672 = AXIS2_PLACEMENT_3D ( 'NONE', #8926, #455, #8664 ) ;
#7673 = EDGE_LOOP ( 'NONE', ( #1, #5565, #4224, #797 ) ) ;
#7674 = CIRCLE ( 'NONE', #2350, 1.000000000000000888 ) ;
#7675 = DIRECTION ( 'NONE',  ( -0.000000000000000000, 1.000000000000000000, 7.930164461608263644E-17 ) ) ;
#7676 = CARTESIAN_POINT ( 'NONE',  ( -19.99508847463048156, 181.5683096734331343, -124.0335439678955112 ) ) ;
#7677 = CARTESIAN_POINT ( 'NONE',  ( -820.5035528205731907, 74.92619343081619832, -105.9719278460594580 ) ) ;
#7678 = FACE_BOUND ( 'NONE', #316, .T. ) ;
#7679 = CARTESIAN_POINT ( 'NONE',  ( -1038.506348936321501, 51.71309463382193883, -146.0307792196451260 ) ) ;
#7680 = ORIENTED_EDGE ( 'NONE', *, *, #2393, .F. ) ;
#7681 = ADVANCED_FACE ( 'NONE', ( #11023 ), #1693, .T. ) ;
#7682 = CARTESIAN_POINT ( 'NONE',  ( -374.9895210541299662, 83.62267570606550748, -144.6251211967523034 ) ) ;
#7683 = DIRECTION ( 'NONE',  ( -1.000000000000000000, -1.186840563529527301E-16, 0.000000000000000000 ) ) ;
#7684 = CARTESIAN_POINT ( 'NONE',  ( -374.4827113483042922, 72.13547865759302624, -107.1640604315173988 ) ) ;
#7685 = DIRECTION ( 'NONE',  ( -1.000000000000000000, 0.000000000000000000, -0.000000000000000000 ) ) ;
#7686 = EDGE_CURVE ( 'NONE', #125, #739, #12083, .T. ) ;
#7687 = ORIENTED_EDGE ( 'NONE', *, *, #5846, .F. ) ;
#7688 = ORIENTED_EDGE ( 'NONE', *, *, #7002, .T. ) ;
#7689 = CARTESIAN_POINT ( 'NONE',  ( -996.0013826475885708, 63.70094029248571132, -96.78565065507963538 ) ) ;
#7690 = CARTESIAN_POINT ( 'NONE',  ( -828.6703486388537385, 79.96407734986419769, -104.7820573548429195 ) ) ;
#7691 = CARTESIAN_POINT ( 'NONE',  ( -954.5446161821218993, 49.54000128949421367, -130.5712005305404091 ) ) ;
#7692 = VERTEX_POINT ( 'NONE', #6386 ) ;
#7693 = EDGE_CURVE ( 'NONE', #7116, #5834, #5451, .T. ) ;
#7694 = CARTESIAN_POINT ( 'NONE',  ( -819.0830098008030973, 80.28235241365214847, -144.6091609974198207 ) ) ;
#7695 = CARTESIAN_POINT ( 'NONE',  ( -383.4612065782806098, 92.42287728680335590, -107.6015166696609668 ) ) ;
#7696 = CARTESIAN_POINT ( 'NONE',  ( -828.6683600116994057, 77.37701618531993120, -154.6440356896530659 ) ) ;
#7697 = VERTEX_POINT ( 'NONE', #1762 ) ;
#7698 = DIRECTION ( 'NONE',  ( 0.000000000000000000, -1.156482317317870246E-16, 1.000000000000000000 ) ) ;
#7699 = APPLICATION_PROTOCOL_DEFINITION ( 'draft international standard', 'automotive_design', 1998, #8448 ) ;
#7700 = EDGE_LOOP ( 'NONE', ( #1712, #11876, #5961, #1447 ) ) ;
#7701 = CARTESIAN_POINT ( 'NONE',  ( -1065.000000000006594, 52.38665522077229042, -118.7903414690683945 ) ) ;
#7702 = CARTESIAN_POINT ( 'NONE',  ( -1065.000000000006594, 112.0000000000007105, -124.6807709998041531 ) ) ;
#7703 = CARTESIAN_POINT ( 'NONE',  ( -157.5000000000000000, 12.00000000000001421, -126.4213562373084301 ) ) ;
#7704 = DIRECTION ( 'NONE',  ( 0.000000000000000000, -1.000000000000000000, 0.000000000000000000 ) ) ;
#7705 = FACE_BOUND ( 'NONE', #11908, .T. ) ;
#7706 = ORIENTED_EDGE ( 'NONE', *, *, #6031, .T. ) ;
#7707 = LINE ( 'NONE', #3939, #8933 ) ;
#7708 = EDGE_LOOP ( 'NONE', ( #9690, #7468 ) ) ;
#7709 = CARTESIAN_POINT ( 'NONE',  ( -795.0000000000070486, 103.3499740386316859, -103.3307627799634218 ) ) ;
#7710 = CARTESIAN_POINT ( 'NONE',  ( -1054.407929976944160, 113.5897173251037628, -130.5712005305405228 ) ) ;
#7711 = DIRECTION ( 'NONE',  ( 0.000000000000000000, 1.000000000000000000, 0.000000000000000000 ) ) ;
#7712 = CARTESIAN_POINT ( 'NONE',  ( -823.7697810748812799, 117.7733807739867871, -124.6807709998041531 ) ) ;
#7713 = VERTEX_POINT ( 'NONE', #9298 ) ;
#7714 = CARTESIAN_POINT ( 'NONE',  ( 8.500000000000010658, 24.00000000000002132, -126.4213562373094959 ) ) ;
#7715 = DIRECTION ( 'NONE',  ( 0.000000000000000000, 0.000000000000000000, 1.000000000000000000 ) ) ;
#7716 = CARTESIAN_POINT ( 'NONE',  ( 87.04832655144112152, 0.000000000000000000, -217.9289243767383368 ) ) ;
#7717 = CARTESIAN_POINT ( 'NONE',  ( -1060.846413679901389, 110.5345601522218146, -136.2353035311979852 ) ) ;
#7718 = CARTESIAN_POINT ( 'NONE',  ( -371.0721991683506644, 105.1220130550264997, -110.4447908282102446 ) ) ;
#7719 = AXIS2_PLACEMENT_3D ( 'NONE', #5099, #8916, #4122 ) ;
#7720 = DIRECTION ( 'NONE',  ( 0.000000000000000000, -1.000000000000000000, 0.000000000000000000 ) ) ;
#7721 = DIRECTION ( 'NONE',  ( -1.000000000000000000, -0.000000000000000000, -0.000000000000000000 ) ) ;
#7722 = EDGE_LOOP ( 'NONE', ( #12009, #10107, #3801, #3763 ) ) ;
#7723 = EDGE_CURVE ( 'NONE', #8695, #3054, #3652, .T. ) ;
#7724 = DIRECTION ( 'NONE',  ( -8.163404592832031500E-17, 1.000000000000000000, 0.000000000000000000 ) ) ;
#7725 = CARTESIAN_POINT ( 'NONE',  ( -952.1456544189259148, 108.1568929870910836, -149.7857175106632042 ) ) ;
#7726 = ADVANCED_FACE ( 'NONE', ( #5760 ), #10565, .T. ) ;
#7727 = FACE_BOUND ( 'NONE', #4399, .T. ) ;
#7728 = ORIENTED_EDGE ( 'NONE', *, *, #11081, .F. ) ;
#7729 = ORIENTED_EDGE ( 'NONE', *, *, #6443, .T. ) ;
#7730 = EDGE_CURVE ( 'NONE', #6181, #9384, #4661, .T. ) ;
#7731 = DIRECTION ( 'NONE',  ( -1.000000000000000000, 0.000000000000000000, 0.000000000000000000 ) ) ;
#7732 = CARTESIAN_POINT ( 'NONE',  ( -381.3400711680802146, 97.95158805382058631, -136.7590353381492889 ) ) ;
#7733 = PLANE ( 'NONE',  #7193 ) ;
#7734 = CARTESIAN_POINT ( 'NONE',  ( -853.7969483066773364, 45.36294356226267865, -149.7857175106635168 ) ) ;
#7735 = AXIS2_PLACEMENT_3D ( 'NONE', #5354, #3557, #1535 ) ;
#7736 = ORIENTED_EDGE ( 'NONE', *, *, #4037, .F. ) ;
#7737 = CARTESIAN_POINT ( 'NONE',  ( -374.7451988284479398, 88.02670150610194355, -153.8963740139208483 ) ) ;
#7738 = FACE_OUTER_BOUND ( 'NONE', #7179, .T. ) ;
#7739 = CARTESIAN_POINT ( 'NONE',  ( -383.5775985103214794, 71.91734269553219860, -107.3587914639481653 ) ) ;
#7740 = CARTESIAN_POINT ( 'NONE',  ( 35.00000000000000000, -4.436643353671145300E-15, 81.78351099501843180 ) ) ;
#7741 = CARTESIAN_POINT ( 'NONE',  ( -1021.607260580477828, 54.24386729702167997, -130.5712005305404659 ) ) ;
#7742 = AXIS2_PLACEMENT_3D ( 'NONE', #4843, #8621, #2071 ) ;
#7743 = ORIENTED_EDGE ( 'NONE', *, *, #11042, .F. ) ;
#7744 = ADVANCED_FACE ( 'NONE', ( #699 ), #769, .T. ) ;
#7745 = VERTEX_POINT ( 'NONE', #9033 ) ;
#7746 = CARTESIAN_POINT ( 'NONE',  ( -150.0000000000000000, 12.00000000000001421, -126.4213562373084301 ) ) ;
#7747 = EDGE_CURVE ( 'NONE', #2602, #9984, #8977, .T. ) ;
#7748 = CARTESIAN_POINT ( 'NONE',  ( -853.9759289228104535, 31.63339360934237021, -107.9061927053328986 ) ) ;
#7749 = CARTESIAN_POINT ( 'NONE',  ( -828.1711263241255665, 81.17408148015046265, -104.6959820179053935 ) ) ;
#7750 = CARTESIAN_POINT ( 'NONE',  ( 3.123963502971610252E-13, 152.0000000000000000, -96.42135623730948168 ) ) ;
#7751 = CARTESIAN_POINT ( 'NONE',  ( -795.0000000000020464, 52.38665522077208436, -130.5712005305402670 ) ) ;
#7752 = EDGE_LOOP ( 'NONE', ( #3043, #2083, #9599, #3922 ) ) ;
#7753 = CARTESIAN_POINT ( 'NONE',  ( -819.4849966174467681, 81.17290644373839825, -144.6655594550755382 ) ) ;
#7754 = CARTESIAN_POINT ( 'NONE',  ( 35.00000000000000000, 152.0000000000000000, 190.3192290001959748 ) ) ;
#7755 = LINE ( 'NONE', #1328, #7799 ) ;
#7756 = CIRCLE ( 'NONE', #3796, 81.99999999999998579 ) ;
#7757 = ORIENTED_EDGE ( 'NONE', *, *, #4748, .T. ) ;
#7758 = APPLICATION_PROTOCOL_DEFINITION ( 'draft international standard', 'automotive_design', 1998, #6132 ) ;
#7759 = VERTEX_POINT ( 'NONE', #12010 ) ;
#7760 = CARTESIAN_POINT ( 'NONE',  ( -1038.719578313838610, 40.52245044769760085, -122.7172756069793707 ) ) ;
#7761 = CARTESIAN_POINT ( 'NONE',  ( -27.99999999999999645, -492.9999999999998863, 27.99999999999999645 ) ) ;
#7762 = FACE_OUTER_BOUND ( 'NONE', #897, .T. ) ;
#7763 = DIRECTION ( 'NONE',  ( 0.000000000000000000, -1.000000000000000000, 0.000000000000000000 ) ) ;
#7764 = EDGE_CURVE ( 'NONE', #8579, #10282, #6814, .T. ) ;
#7765 = CARTESIAN_POINT ( 'NONE',  ( -232.4999999999999716, 24.00000000000000711, -126.4213562373078190 ) ) ;
#7766 = CARTESIAN_POINT ( 'NONE',  ( -19.87519864879852349, 178.8871479037923393, -126.9115732480538838 ) ) ;
#7767 = VERTEX_POINT ( 'NONE', #6203 ) ;
#7768 = CARTESIAN_POINT ( 'NONE',  ( -374.5759732026825759, 74.23177511559134700, -153.3650736963693078 ) ) ;
#7769 = AXIS2_PLACEMENT_3D ( 'NONE', #2512, #2706, #1587 ) ;
#7770 =( LENGTH_UNIT ( ) NAMED_UNIT ( * ) SI_UNIT ( .MILLI., .METRE. ) );
#7771 = EDGE_LOOP ( 'NONE', ( #10849, #1651, #11405, #4226 ) ) ;
#7772 = CARTESIAN_POINT ( 'NONE',  ( -1046.909978542194949, 84.99913997988220160, -95.06748246948046699 ) ) ;
#7773 = ORIENTED_EDGE ( 'NONE', *, *, #733, .F. ) ;
#7774 = LINE ( 'NONE', #7841, #4908 ) ;
#7775 = CARTESIAN_POINT ( 'NONE',  ( 1.874378101782966050E-12, -6.000000000000005329, 53.57864376269050410 ) ) ;
#7776 = AXIS2_PLACEMENT_3D ( 'NONE', #164, #1914, #9453 ) ;
#7777 = VECTOR ( 'NONE', #11201, 1000.000000000000000 ) ;
#7778 = CARTESIAN_POINT ( 'NONE',  ( -904.2101318206010774, 125.2895275102983419, -122.7172756069790580 ) ) ;
#7779 = ORIENTED_EDGE ( 'NONE', *, *, #3264, .F. ) ;
#7780 = DIRECTION ( 'NONE',  ( 0.000000000000000000, -1.156482317317870246E-16, 1.000000000000000000 ) ) ;
#7781 = CARTESIAN_POINT ( 'NONE',  ( -820.7717470982031500, 82.64484858469192829, -104.6903222377186893 ) ) ;
#7782 = CARTESIAN_POINT ( 'NONE',  ( 0.000000000000000000, 0.000000000000000000, -224.6807709998039968 ) ) ;
#7783 = CARTESIAN_POINT ( 'NONE',  ( -1024.848917040341576, 116.4131098345822437, -136.2353035311980420 ) ) ;
#7784 = CARTESIAN_POINT ( 'NONE',  ( -380.6764949106236600, 99.29952767699337812, -114.6234865369922034 ) ) ;
#7785 = CARTESIAN_POINT ( 'NONE',  ( -30.00000000000000000, -6.000000000000000000, -30.00000000000000000 ) ) ;
#7786 = ORIENTED_EDGE ( 'NONE', *, *, #5852, .F. ) ;
#7787 = CIRCLE ( 'NONE', #4422, 7.500000000000007105 ) ;
#7788 = CARTESIAN_POINT ( 'NONE',  ( -974.1288507787421622, 124.2142274477007078, -126.6442663926288787 ) ) ;
#7789 = AXIS2_PLACEMENT_3D ( 'NONE', #9241, #12093, #7698 ) ;
#7790 = CIRCLE ( 'NONE', #2449, 7.500000000000007105 ) ;
#7791 = CARTESIAN_POINT ( 'NONE',  ( -126.4213562373094959, -494.9999999999998863, 2.255140518769849223E-14 ) ) ;
#7792 = CARTESIAN_POINT ( 'NONE',  ( -1025.595388641371756, 103.7168792382127975, -149.7857175106636021 ) ) ;
#7793 = DIRECTION ( 'NONE',  ( 0.000000000000000000, 0.000000000000000000, 1.000000000000000000 ) ) ;
#7794 = PLANE ( 'NONE',  #3192 ) ;
#7795 = ORIENTED_EDGE ( 'NONE', *, *, #2615, .T. ) ;
#7796 = APPLICATION_CONTEXT ( 'automotive_design' ) ;
#7797 = VERTEX_POINT ( 'NONE', #8181 ) ;
#7798 = ADVANCED_FACE ( 'NONE', ( #9971 ), #1745, .T. ) ;
#7799 = VECTOR ( 'NONE', #4906, 999.9999999999998863 ) ;
#7800 = CIRCLE ( 'NONE', #11554, 7.500000000000020428 ) ;
#7801 = FACE_BOUND ( 'NONE', #2192, .T. ) ;
#7802 = CARTESIAN_POINT ( 'NONE',  ( -928.2641150402240555, 65.00826535581498433, -141.4553492942759476 ) ) ;
#7803 = CARTESIAN_POINT ( 'NONE',  ( -37.49999999999999289, 12.00000000000001776, -126.4213562373092685 ) ) ;
#7804 = ORIENTED_EDGE ( 'NONE', *, *, #9627, .T. ) ;
#7805 = CARTESIAN_POINT ( 'NONE',  ( -374.0261869715998273, 70.33727264991432548, -151.5753310962235503 ) ) ;
#7806 = DIRECTION ( 'NONE',  ( -1.186840563529527301E-16, 1.000000000000000000, -0.000000000000000000 ) ) ;
#7807 = ORIENTED_EDGE ( 'NONE', *, *, #2610, .T. ) ;
#7808 = B_SPLINE_CURVE_WITH_KNOTS ( 'NONE', 3,
 ( #10015, #8105, #11931, #5308, #6363, #3510 ),
 .UNSPECIFIED., .F., .F.,
 ( 4, 2, 4 ),
 ( 2.380730968222468785E-07, 0.002629065763328365234, 0.005257893453559908843 ),
 .UNSPECIFIED. ) ;
#7809 = CIRCLE ( 'NONE', #296, 5.999999999999999112 ) ;
#7810 = ORIENTED_EDGE ( 'NONE', *, *, #3087, .T. ) ;
#7811 = ORIENTED_EDGE ( 'NONE', *, *, #9267, .T. ) ;
#7812 = CYLINDRICAL_SURFACE ( 'NONE', #10388, 175.0000000000000284 ) ;
#7813 = CARTESIAN_POINT ( 'NONE',  ( -1013.844210246976672, 57.79547239392030633, -107.9061927053327423 ) ) ;
#7814 = CYLINDRICAL_SURFACE ( 'NONE', #9268, 7.500000000000020428 ) ;
#7815 = ADVANCED_FACE ( 'NONE', ( #5264 ), #5328, .F. ) ;
#7816 = ORIENTED_EDGE ( 'NONE', *, *, #860, .T. ) ;
#7817 = AXIS2_PLACEMENT_3D ( 'NONE', #11574, #7866, #9771 ) ;
#7818 = DIRECTION ( 'NONE',  ( -1.000000000000000000, 0.000000000000000000, 0.000000000000000000 ) ) ;
#7819 = VERTEX_POINT ( 'NONE', #11454 ) ;
#7820 = CARTESIAN_POINT ( 'NONE',  ( -821.6140151324020735, 74.17967406092559202, -154.6554517456385440 ) ) ;
#7821 = EDGE_LOOP ( 'NONE', ( #4506, #3975, #11396, #10570 ) ) ;
#7822 = SHAPE_DEFINITION_REPRESENTATION ( #9800, #12149 ) ;
#7823 = ORIENTED_EDGE ( 'NONE', *, *, #2018, .F. ) ;
#7824 = CARTESIAN_POINT ( 'NONE',  ( -1014.132585063772353, 52.13780504951625261, -122.7172756069792428 ) ) ;
#7825 = CARTESIAN_POINT ( 'NONE',  ( -89.99999999999998579, 24.00000000000001421, -126.4213562373088564 ) ) ;
#7826 = CARTESIAN_POINT ( 'NONE',  ( 1.561981751485805177E-12, -6.000000000000005329, 23.57864376269050410 ) ) ;
#7827 = CIRCLE ( 'NONE', #5241, 1.000000000000000888 ) ;
#7828 = CARTESIAN_POINT ( 'NONE',  ( -974.4564103291414767, 111.0951925441806480, -103.3307627799632371 ) ) ;
#7829 = CARTESIAN_POINT ( 'NONE',  ( 9.381075359908434252E-13, 0.000000000000000000, -43.92135623730950300 ) ) ;
#7830 = DIRECTION ( 'NONE',  ( -0.000000000000000000, 1.000000000000000000, -0.000000000000000000 ) ) ;
#7831 = VERTEX_POINT ( 'NONE', #5583 ) ;
#7832 = PRODUCT_DEFINITION_SHAPE ( 'NONE', 'NONE',  #12249 ) ;
#7833 = DIRECTION ( 'NONE',  ( -0.000000000000000000, 1.000000000000000000, 7.930164461608263644E-17 ) ) ;
#7834 = ADVANCED_FACE ( 'NONE', ( #4608 ), #1017, .F. ) ;
#7835 = ORIENTED_EDGE ( 'NONE', *, *, #7686, .F. ) ;
#7836 = CARTESIAN_POINT ( 'NONE',  ( -822.2439855206088168, 97.57287547056382948, -99.57582448894494576 ) ) ;
#7837 = AXIS2_PLACEMENT_3D ( 'NONE', #7196, #10965, #333 ) ;
#7838 = ORIENTED_EDGE ( 'NONE', *, *, #2710, .T. ) ;
#7839 = CARTESIAN_POINT ( 'NONE',  ( -852.8274699693135972, 120.9962006285028906, -130.5712005305406933 ) ) ;
#7840 = CARTESIAN_POINT ( 'NONE',  ( -1065.000000000002501, 109.8950841424301359, -136.2353035311980136 ) ) ;
#7841 = CARTESIAN_POINT ( 'NONE',  ( -955.0000000000038654, 62.00000000000019185, -124.6807709998041815 ) ) ;
#7842 = EDGE_CURVE ( 'NONE', #11231, #1969, #1080, .T. ) ;
#7843 = LINE ( 'NONE', #5045, #7339 ) ;
#7844 = CARTESIAN_POINT ( 'NONE',  ( -951.4444194419894529, 124.5703232071642503, -118.7903414690678829 ) ) ;
#7845 = ORIENTED_EDGE ( 'NONE', *, *, #2583, .F. ) ;
#7846 = AXIS2_PLACEMENT_3D ( 'NONE', #11092, #3475, #3534 ) ;
#7847 = CARTESIAN_POINT ( 'NONE',  ( 126.4213562373094959, -494.9999999999998863, 7.500000000000006217 ) ) ;
#7848 = DIRECTION ( 'NONE',  ( -0.000000000000000000, -1.000000000000000000, -0.000000000000000000 ) ) ;
#7849 = CARTESIAN_POINT ( 'NONE',  ( -951.9057582426059980, 113.9552214607316216, -146.0307792196438754 ) ) ;
#7850 = EDGE_CURVE ( 'NONE', #5193, #2379, #8554, .T. ) ;
#7851 = CARTESIAN_POINT ( 'NONE',  ( 20.75416591570629876, 179.5558320214803132, -123.4493688440947921 ) ) ;
#7852 = DIRECTION ( 'NONE',  ( 0.000000000000000000, 0.000000000000000000, 1.000000000000000000 ) ) ;
#7853 = ORIENTED_EDGE ( 'NONE', *, *, #3828, .T. ) ;
#7854 = DIRECTION ( 'NONE',  ( 0.000000000000000000, 0.000000000000000000, 1.000000000000000000 ) ) ;
#7855 = CARTESIAN_POINT ( 'NONE',  ( 126.4213562373094959, -492.9999999999998863, -7.500000000000019540 ) ) ;
#7856 = DIRECTION ( 'NONE',  ( 0.000000000000000000, 0.000000000000000000, -1.000000000000000000 ) ) ;
#7857 = CARTESIAN_POINT ( 'NONE',  ( -1014.170783943998003, 114.7803637426474808, -141.4553492942763171 ) ) ;
#7858 = AXIS2_PLACEMENT_3D ( 'NONE', #188, #3970, #10703 ) ;
#7859 = DIRECTION ( 'NONE',  ( 3.061276722312011504E-17, -1.000000000000000000, -0.000000000000000000 ) ) ;
#7860 = ORIENTED_EDGE ( 'NONE', *, *, #1645, .F. ) ;
#7861 = CARTESIAN_POINT ( 'NONE',  ( -7.499999999999994671, -9.213203435596451385, -126.4213562373094959 ) ) ;
#7862 = ORIENTED_EDGE ( 'NONE', *, *, #4202, .T. ) ;
#7863 = CARTESIAN_POINT ( 'NONE',  ( 19.99397847396136996, 178.8651426120512724, -123.9853605248128474 ) ) ;
#7864 = CARTESIAN_POINT ( 'NONE',  ( -384.7284696814416520, 86.42946640087690469, -144.1932104012986429 ) ) ;
#7865 = CARTESIAN_POINT ( 'NONE',  ( -853.8938961404190877, 37.86297855175782701, -146.0307792196449554 ) ) ;
#7866 = DIRECTION ( 'NONE',  ( -0.000000000000000000, -1.000000000000000000, -0.000000000000000000 ) ) ;
#7867 = VECTOR ( 'NONE', #8153, 1000.000000000000000 ) ;
#7868 = CARTESIAN_POINT ( 'NONE',  ( -374.8244134398003098, 87.00545050162834571, -154.1417378514361758 ) ) ;
#7869 = LINE ( 'NONE', #373, #1867 ) ;
#7870 = CARTESIAN_POINT ( 'NONE',  ( -821.6148272622868944, 74.17911137529775090, -94.70610353401345094 ) ) ;
#7871 = B_SPLINE_CURVE_WITH_KNOTS ( 'NONE', 3,
 ( #3673, #7446, #2756, #11229, #1830, #4902 ),
 .UNSPECIFIED., .F., .F.,
 ( 4, 2, 4 ),
 ( 0.000000000000000000, 0.003279474516629658862, 0.006558949033259317725 ),
 .UNSPECIFIED. ) ;
#7872 = ORIENTED_EDGE ( 'NONE', *, *, #340, .T. ) ;
#7873 = CARTESIAN_POINT ( 'NONE',  ( -1028.454949082223038, 53.01113643315406421, -136.2353035311987810 ) ) ;
#7874 = CIRCLE ( 'NONE', #5901, 7.500000000000007105 ) ;
#7875 = ORIENTED_EDGE ( 'NONE', *, *, #3978, .F. ) ;
#7876 = DIRECTION ( 'NONE',  ( 0.000000000000000000, 0.000000000000000000, 1.000000000000000000 ) ) ;
#7877 = CARTESIAN_POINT ( 'NONE',  ( -1028.581275045472694, 51.02622020309998163, -118.7903414690682240 ) ) ;
#7878 = CARTESIAN_POINT ( 'NONE',  ( -19.98117600975061592, 182.6057245623286462, -125.5759384559340077 ) ) ;
#7879 = EDGE_LOOP ( 'NONE', ( #2395, #2313, #7887, #10905 ) ) ;
#7880 = CARTESIAN_POINT ( 'NONE',  ( -210.0000000000000000, -9.213203435596478030, -126.4213562373080180 ) ) ;
#7881 = CIRCLE ( 'NONE', #5896, 7.500000000000012434 ) ;
#7882 = CARTESIAN_POINT ( 'NONE',  ( -154.5043356068770493, 12.00000000000000000, -109.5666613060160586 ) ) ;
#7883 = VERTEX_POINT ( 'NONE', #10522 ) ;
#7884 = DIRECTION ( 'NONE',  ( 0.000000000000000000, -1.000000000000000000, -7.930164461608263644E-17 ) ) ;
#7885 = ORIENTED_EDGE ( 'NONE', *, *, #1884, .F. ) ;
#7886 =( BOUNDED_SURFACE ( )  B_SPLINE_SURFACE ( 3, 2, ( 
 ( #6355, #6295, #8155 ),
 ( #4383, #1854, #3698 ),
 ( #10065, #1596, #7476 ),
 ( #8353, #1661, #9073 ),
 ( #5358, #4644, #10193 ),
 ( #11254, #3560, #3630 ),
 ( #870, #1733, #7415 ),
 ( #7351, #9134, #11056 ),
 ( #5421, #608, #11923 ),
 ( #11191, #4513, #2582 ),
 ( #3444, #674, #4449 ),
 ( #11122, #8421, #12183 ),
 ( #10994, #11985, #2713 ),
 ( #1791, #8225, #5493 ),
 ( #7227, #2779, #10258 ),
 ( #6543, #10126, #6486 ),
 ( #8292, #2521, #3502 ),
 ( #7291, #9200, #12048 ),
 ( #2647, #6423, #9266 ),
 ( #808, #4580, #12117 ),
 ( #5556, #10313, #9330 ),
 ( #10797, #2334, #5222 ),
 ( #459, #4254, #8023 ),
 ( #527, #6161, #9927 ),
 ( #10360, #3544, #11173 ),
 ( #6471, #30, #11105 ),
 ( #9498, #6654, #1040 ),
 ( #8466, #9379, #9314 ),
 ( #1714, #5664, #10243 ),
 ( #5541, #11350, #5473 ) ),
 .UNSPECIFIED., .F., .F., .F. ) 
 B_SPLINE_SURFACE_WITH_KNOTS ( ( 4, 2, 2, 2, 2, 2, 2, 2, 2, 2, 2, 2, 2, 2, 4 ),
 ( 3, 3 ),
 ( 0.007889744914357701283, 0.008875963028655821374, 0.009369072085804883154, 0.009862181142953943200, 0.01035529020010300325, 0.01084839925725206503, 0.01134150831440112507, 0.01183461737155018512, 0.01232772642869924516, 0.01282083548584830521, 0.01380705360014642703, 0.01430016265729548708, 0.01479327171444454886, 0.01528638077159360890, 0.01577948982874266895 ),
 ( 0.000000000000000000, 1.000000000000000000 ),
 .UNSPECIFIED. ) 
 GEOMETRIC_REPRESENTATION_ITEM ( )  RATIONAL_B_SPLINE_SURFACE ( (
 ( 1.000000000000000000, 0.7788034628477763510, 1.000000000000000000),
 ( 1.000000000000000000, 0.7721230128607156074, 1.000000000000000000),
 ( 1.000000000000000000, 0.7637060791568476281, 1.000000000000000000),
 ( 1.000000000000000000, 0.7496516620472627457, 1.000000000000000000),
 ( 1.000000000000000000, 0.7447560477940591284, 1.000000000000000000),
 ( 1.000000000000000000, 0.7349957282090778810, 1.000000000000000000),
 ( 1.000000000000000000, 0.7300720695073790178, 1.000000000000000000),
 ( 1.000000000000000000, 0.7203457075533885590, 1.000000000000000000),
 ( 1.000000000000000000, 0.7156722358407558993, 1.000000000000000000),
 ( 1.000000000000000000, 0.7067788860353876323, 1.000000000000000000),
 ( 1.000000000000000000, 0.7025175898284636844, 1.000000000000000000),
 ( 1.000000000000000000, 0.6947521172562991509, 1.000000000000000000),
 ( 1.000000000000000000, 0.6912534286752571866, 1.000000000000000000),
 ( 1.000000000000000000, 0.6849888440347751128, 1.000000000000000000),
 ( 1.000000000000000000, 0.6822120470311171525, 1.000000000000000000),
 ( 1.000000000000000000, 0.6775429675546015273, 1.000000000000000000),
 ( 1.000000000000000000, 0.6756152869907889880, 1.000000000000000000),
 ( 1.000000000000000000, 0.6724212228960821935, 1.000000000000000000),
 ( 1.000000000000000000, 0.6711767660106030542, 1.000000000000000000),
 ( 1.000000000000000000, 0.6682954301978540901, 1.000000000000000000),
 ( 1.000000000000000000, 0.6674300803999402287, 1.000000000000000000),
 ( 1.000000000000000000, 0.6667725974591163229, 1.000000000000000000),
 ( 1.000000000000000000, 0.6666584258004638608, 1.000000000000000000),
 ( 1.000000000000000000, 0.6665746734483880553, 1.000000000000000000),
 ( 1.000000000000000000, 0.6666022109305942411, 1.000000000000000000),
 ( 1.000000000000000000, 0.6668181847376934979, 1.000000000000000000),
 ( 1.000000000000000000, 0.6670097042269241827, 1.000000000000000000),
 ( 1.000000000000000000, 0.6676556552395226385, 1.000000000000000000),
 ( 1.000000000000000000, 0.6681120711471668638, 1.000000000000000000),
 ( 1.000000000000000000, 0.6687969305523246977, 1.000000000000000000) ) ) 
 REPRESENTATION_ITEM ( '' )  SURFACE ( )  );
#7887 = ORIENTED_EDGE ( 'NONE', *, *, #2424, .T. ) ;
#7888 = CARTESIAN_POINT ( 'NONE',  ( -1017.158871447982051, 53.64146012065780411, -122.7172756069791717 ) ) ;
#7889 = ADVANCED_FACE ( 'NONE', ( #9357 ), #9296, .F. ) ;
#7890 = DIRECTION ( 'NONE',  ( -1.000000000000000000, -0.000000000000000000, -0.000000000000000000 ) ) ;
#7891 = DIRECTION ( 'NONE',  ( 1.000000000000000000, 0.000000000000000000, 0.000000000000000000 ) ) ;
#7892 = EDGE_CURVE ( 'NONE', #10902, #11947, #9437, .T. ) ;
#7893 = CIRCLE ( 'NONE', #10454, 7.500000000000007105 ) ;
#7894 = CARTESIAN_POINT ( 'NONE',  ( 57.50000000000000000, 0.000000000000000000, 5.035999999999999588 ) ) ;
#7895 = CARTESIAN_POINT ( 'NONE',  ( -1055.176328965296989, 98.13059730676610570, -99.57582448894517313 ) ) ;
#7896 = CARTESIAN_POINT ( 'NONE',  ( 7.500000000000000000, 10.39230484541326938, 0.000000000000000000 ) ) ;
#7897 = ORIENTED_EDGE ( 'NONE', *, *, #1790, .F. ) ;
#7898 = DIRECTION ( 'NONE',  ( 0.000000000000000000, -1.156482317317870246E-16, 1.000000000000000000 ) ) ;
#7899 = AXIS2_PLACEMENT_3D ( 'NONE', #6714, #9500, #2090 ) ;
#7900 = EDGE_LOOP ( 'NONE', ( #927, #11497, #3578, #2584 ) ) ;
#7901 = CARTESIAN_POINT ( 'NONE',  ( -927.2951026182247460, 99.13268410970638911, -95.06748246948001224 ) ) ;
#7902 = EDGE_LOOP ( 'NONE', ( #3961, #6635, #4982, #11844 ) ) ;
#7903 = CARTESIAN_POINT ( 'NONE',  ( -1037.348432443219735, 116.4729352038311987, -130.5712005305406080 ) ) ;
#7904 = CARTESIAN_POINT ( 'NONE',  ( -1030.931480980266770, 117.9615145441171933, -126.6442663926290777 ) ) ;
#7905 = CARTESIAN_POINT ( 'NONE',  ( 19.89852930574608791, 181.2981474642644741, -122.6658827718632949 ) ) ;
#7906 = ADVANCED_FACE ( 'NONE', ( #12206 ), #8503, .F. ) ;
#7907 = CARTESIAN_POINT ( 'NONE',  ( -974.1454360724308117, 123.6012932931490127, -118.7903414690677835 ) ) ;
#7908 = CARTESIAN_POINT ( 'NONE',  ( 7.500000000000000000, 0.000000000000000000, 0.000000000000000000 ) ) ;
#7909 = DIRECTION ( 'NONE',  ( 0.000000000000000000, 0.000000000000000000, 1.000000000000000000 ) ) ;
#7910 = CARTESIAN_POINT ( 'NONE',  ( -87.04832655144203102, 0.000000000000000000, -217.9289243767376831 ) ) ;
#7911 = CARTESIAN_POINT ( 'NONE',  ( -379.7921418149325063, 63.07164944986214294, -118.2218589047913611 ) ) ;
#7912 = CARTESIAN_POINT ( 'NONE',  ( -380.0568384841039915, 100.4584982090781295, -116.9531293578063327 ) ) ;
#7913 = SURFACE_STYLE_USAGE ( .BOTH. , #10743 ) ;
#7914 = CARTESIAN_POINT ( 'NONE',  ( -823.8285638327238303, 78.67432280806536937, -89.68077099980398259 ) ) ;
#7915 = ORIENTED_EDGE ( 'NONE', *, *, #7068, .T. ) ;
#7916 = DIRECTION ( 'NONE',  ( -0.000000000000000000, 1.000000000000000000, 0.000000000000000000 ) ) ;
#7917 = CARTESIAN_POINT ( 'NONE',  ( -795.0000000000035243, 112.0000000000008953, -126.6442663926293477 ) ) ;
#7918 = CYLINDRICAL_SURFACE ( 'NONE', #9100, 7.500000000000012434 ) ;
#7919 = CARTESIAN_POINT ( 'NONE',  ( -1014.382386707152364, 110.5980896718283759, -146.0307792196445291 ) ) ;
#7920 = CARTESIAN_POINT ( 'NONE',  ( -305.0000000000000568, 81.99999999999995737, -89.68077099980384048 ) ) ;
#7921 = ORIENTED_EDGE ( 'NONE', *, *, #6377, .T. ) ;
#7922 = EDGE_CURVE ( 'NONE', #9588, #7116, #4104, .T. ) ;
#7923 = EDGE_LOOP ( 'NONE', ( #3540, #8900, #8474, #2649 ) ) ;
#7924 = CARTESIAN_POINT ( 'NONE',  ( -381.8376525299339619, 67.14791246521063783, -138.0876920893665272 ) ) ;
#7925 = CARTESIAN_POINT ( 'NONE',  ( -819.8405841167685821, 75.64117232352727171, -143.6450765909193876 ) ) ;
#7926 = CARTESIAN_POINT ( 'NONE',  ( 1.249585401188644101E-12, 12.00000000000000000, 1.078643762690514762 ) ) ;
#7927 = DIRECTION ( 'NONE',  ( 0.000000000000000000, -1.000000000000000000, -1.850371707708592551E-14 ) ) ;
#7928 = DIRECTION ( 'NONE',  ( 0.000000000000000000, 0.000000000000000000, -1.000000000000000000 ) ) ;
#7929 = FILL_AREA_STYLE_COLOUR ( '', #8254 ) ;
#7930 = CARTESIAN_POINT ( 'NONE',  ( -997.4616017999776432, 44.34671234275830187, -141.4553492942759476 ) ) ;
#7931 = ORIENTED_EDGE ( 'NONE', *, *, #782, .T. ) ;
#7932 = PRODUCT ( 'pin to fix handle', 'pin to fix handle', '', ( #11342 ) ) ;
#7933 = ORIENTED_EDGE ( 'NONE', *, *, #8854, .T. ) ;
#7934 = DIRECTION ( 'NONE',  ( 0.000000000000000000, 1.000000000000000000, 0.000000000000000000 ) ) ;
#7935 = CIRCLE ( 'NONE', #2596, 9.000000000000000000 ) ;
#7936 = CARTESIAN_POINT ( 'NONE',  ( -1025.976186494711783, 52.68972726728017619, -122.7172756069792428 ) ) ;
#7937 = ORIENTED_EDGE ( 'NONE', *, *, #1560, .T. ) ;
#7938 = CARTESIAN_POINT ( 'NONE',  ( -827.1323880180814285, 82.44176594610610209, -95.11041087168378283 ) ) ;
#7939 = CARTESIAN_POINT ( 'NONE',  ( 35.00000000000000000, 81.99999999999998579, 272.3192290001959464 ) ) ;
#7940 = ORIENTED_EDGE ( 'NONE', *, *, #4216, .T. ) ;
#7941 = CARTESIAN_POINT ( 'NONE',  ( -828.7959811946850550, 78.01751516534540087, -154.6175107292156952 ) ) ;
#7942 = EDGE_LOOP ( 'NONE', ( #10259, #3867, #8871, #6926 ) ) ;
#7943 = ORIENTED_EDGE ( 'NONE', *, *, #6229, .F. ) ;
#7944 = CARTESIAN_POINT ( 'NONE',  ( -901.8785362142587019, 56.55314031071017666, -122.7172756069789017 ) ) ;
#7945 = CARTESIAN_POINT ( 'NONE',  ( -67.49999999999998579, 24.00000000000001421, -126.4213562373090696 ) ) ;
#7946 = DIRECTION ( 'NONE',  ( -0.000000000000000000, -1.000000000000000000, -0.000000000000000000 ) ) ;
#7947 = UNCERTAINTY_MEASURE_WITH_UNIT (LENGTH_MEASURE( 1.000000000000000082E-05 ), #4651, 'distance_accuracy_value', 'NONE');
#7948 = FACE_OUTER_BOUND ( 'NONE', #11646, .T. ) ;
#7949 = CARTESIAN_POINT ( 'NONE',  ( -1019.017691546883157, 99.44610047464911418, -96.78565065507929432 ) ) ;
#7950 = CARTESIAN_POINT ( 'NONE',  ( 4.255174644013695128E-15, 25.00000000000002132, -126.4213562373094959 ) ) ;
#7951 = VECTOR ( 'NONE', #1264, 1000.000000000000000 ) ;
#7952 = EDGE_CURVE ( 'NONE', #3290, #9727, #3712, .T. ) ;
#7953 = ORIENTED_EDGE ( 'NONE', *, *, #5756, .T. ) ;
#7954 = CARTESIAN_POINT ( 'NONE',  ( 126.4213562373094959, 12.00000000000000000, -6.938893903907228378E-15 ) ) ;
#7955 = DIRECTION ( 'NONE',  ( 1.000000000000000000, 0.000000000000000000, 0.000000000000000000 ) ) ;
#7956 = ADVANCED_FACE ( 'NONE', ( #8384 ), #3729, .F. ) ;
#7957 = FILL_AREA_STYLE_COLOUR ( '', #7014 ) ;
#7958 = ORIENTED_EDGE ( 'NONE', *, *, #6679, .T. ) ;
#7959 = CARTESIAN_POINT ( 'NONE',  ( -1056.106496161727136, 78.18408418063160070, -94.48732055948630659 ) ) ;
#7960 = DIRECTION ( 'NONE',  ( -0.000000000000000000, -7.930164461608263644E-17, 1.000000000000000000 ) ) ;
#7961 = CARTESIAN_POINT ( 'NONE',  ( -904.2101318206000542, 125.2895275102983419, -126.6442663926292340 ) ) ;
#7962 = DIRECTION ( 'NONE',  ( 0.000000000000000000, 0.000000000000000000, -1.000000000000000000 ) ) ;
#7963 = B_SPLINE_CURVE_WITH_KNOTS ( 'NONE', 3,
 ( #2279, #2392, #6933, #10643, #6005, #2293 ),
 .UNSPECIFIED., .F., .F.,
 ( 4, 2, 4 ),
 ( 0.03045342004259713950, 0.03308352806736652996, 0.03571363609213591694 ),
 .UNSPECIFIED. ) ;
#7964 = DIRECTION ( 'NONE',  ( -8.163404592832031500E-17, 1.000000000000000000, 0.000000000000000000 ) ) ;
#7965 = CARTESIAN_POINT ( 'NONE',  ( -240.0000000000000000, -9.213203435596478030, -126.4213562373078190 ) ) ;
#7966 = CARTESIAN_POINT ( 'NONE',  ( -19.92026566182175884, 181.6832013291224541, -122.8938598614162174 ) ) ;
#7967 = AXIS2_PLACEMENT_3D ( 'NONE', #6712, #7579, #2891 ) ;
#7968 = CARTESIAN_POINT ( 'NONE',  ( -828.8285638327203060, 78.83536470144997566, -104.9320557148177926 ) ) ;
#7969 = CARTESIAN_POINT ( 'NONE',  ( -112.4999999999999858, 139.9999999999999716, -126.4213562373086575 ) ) ;
#7970 = EDGE_CURVE ( 'NONE', #5145, #4637, #341, .T. ) ;
#7971 = EDGE_CURVE ( 'NONE', #11480, #5193, #4728, .T. ) ;
#7972 = CARTESIAN_POINT ( 'NONE',  ( -818.8610632455868199, 79.33015038929181628, -94.77164022161367996 ) ) ;
#7973 = FACE_BOUND ( 'NONE', #5380, .T. ) ;
#7974 = VERTEX_POINT ( 'NONE', #5647 ) ;
#7975 = DIRECTION ( 'NONE',  ( 3.061276722312011504E-17, -1.000000000000000000, 0.000000000000000000 ) ) ;
#7976 = DIRECTION ( 'NONE',  ( 0.000000000000000000, -1.156482317317870246E-16, 1.000000000000000000 ) ) ;
#7977 = CIRCLE ( 'NONE', #449, 7.500000000000007994 ) ;
#7978 = DIRECTION ( 'NONE',  ( 0.7071067811865477948, 0.000000000000000000, 0.7071067811865473507 ) ) ;
#7979 = ORIENTED_EDGE ( 'NONE', *, *, #7723, .F. ) ;
#7980 = ORIENTED_EDGE ( 'NONE', *, *, #3742, .F. ) ;
#7981 = CARTESIAN_POINT ( 'NONE',  ( 20.71882545568003664, 180.2153781204678182, -123.3020207091857401 ) ) ;
#7982 = CARTESIAN_POINT ( 'NONE',  ( -381.3383124606481260, 66.03027902319438169, -136.7757352781387112 ) ) ;
#7983 = CARTESIAN_POINT ( 'NONE',  ( -819.1462522098594263, 76.91297450996670193, -144.0236343770281451 ) ) ;
#7984 = VECTOR ( 'NONE', #1815, 1000.000000000000000 ) ;
#7985 = VECTOR ( 'NONE', #5245, 1000.000000000000000 ) ;
#7986 = CARTESIAN_POINT ( 'NONE',  ( -372.6862240691809234, 99.87440285508435522, -146.7032139785486038 ) ) ;
#7987 = DIRECTION ( 'NONE',  ( 0.000000000000000000, 0.000000000000000000, 1.000000000000000000 ) ) ;
#7988 = CARTESIAN_POINT ( 'NONE',  ( -371.5046744491019126, 60.13769991414361726, -107.9593700007184651 ) ) ;
#7989 = ADVANCED_FACE ( 'NONE', ( #2743 ), #9420, .F. ) ;
#7991 = EDGE_CURVE ( 'NONE', #4712, #7498, #2327, .T. ) ;
#7990 = PRESENTATION_STYLE_ASSIGNMENT (( #9660 ) ) ;
#7992 = ORIENTED_EDGE ( 'NONE', *, *, #639, .F. ) ;
#7993 = CARTESIAN_POINT ( 'NONE',  ( -1016.402231264567945, 68.39482517277122042, -149.7857175106636589 ) ) ;
#7994 = ORIENTED_EDGE ( 'NONE', *, *, #11, .F. ) ;
#7995 = EDGE_CURVE ( 'NONE', #2379, #10867, #73, .T. ) ;
#7996 = AXIS2_PLACEMENT_3D ( 'NONE', #5215, #6099, #450 ) ;
#7997 = AXIS2_PLACEMENT_3D ( 'NONE', #3036, #6806, #431 ) ;
#7998 = EDGE_LOOP ( 'NONE', ( #4217, #3504 ) ) ;
#7999 = CARTESIAN_POINT ( 'NONE',  ( -1038.664246639915291, 43.28664065472965206, -113.1262384684093405 ) ) ;
#8000 = CARTESIAN_POINT ( 'NONE',  ( -828.0764331662031736, 81.31668519957902674, -94.98799056389854911 ) ) ;
#8001 = DIRECTION ( 'NONE',  ( -8.163404592832030268E-17, 1.000000000000000000, -0.000000000000000000 ) ) ;
#8002 = ORIENTED_EDGE ( 'NONE', *, *, #9910, .T. ) ;
#8003 = EDGE_CURVE ( 'NONE', #2829, #11444, #11393, .T. ) ;
#8004 = AXIS2_PLACEMENT_3D ( 'NONE', #7381, #3530, #7322 ) ;
#8005 = AXIS2_PLACEMENT_3D ( 'NONE', #8596, #6556, #5627 ) ;
#8006 = ORIENTED_EDGE ( 'NONE', *, *, #10735, .T. ) ;
#8007 = CARTESIAN_POINT ( 'NONE',  ( 4.216865464401061553E-15, 168.0000000000000000, -124.6807709998038405 ) ) ;
#8008 = MANIFOLD_SOLID_BREP ( 'Cut-Extrude4[2]', #7085 ) ;
#8009 = VECTOR ( 'NONE', #7144, 999.9999999999998863 ) ;
#8010 = CARTESIAN_POINT ( 'NONE',  ( -903.4746773471185861, 104.0883302344921475, -96.78565065507889642 ) ) ;
#8011 = CARTESIAN_POINT ( 'NONE',  ( -19.98192996636583274, 177.7975057939641772, -125.5577353981673099 ) ) ;
#8012 = CARTESIAN_POINT ( 'NONE',  ( -374.7795003443170572, 87.57921835826481072, -95.35916363615964997 ) ) ;
#8013 = B_SPLINE_CURVE_WITH_KNOTS ( 'NONE', 3,
 ( #4690, #8465, #5404, #7272, #8274, #3683 ),
 .UNSPECIFIED., .F., .F.,
 ( 4, 2, 4 ),
 ( 0.004972348860735044569, 0.005379997031218691772, 0.005787645201702338975 ),
 .UNSPECIFIED. ) ;
#8014 = VERTEX_POINT ( 'NONE', #11701 ) ;
#8015 = DIRECTION ( 'NONE',  ( 3.061276722312011504E-17, -1.000000000000000000, 0.000000000000000000 ) ) ;
#8016 = CARTESIAN_POINT ( 'NONE',  ( -21.06809339192879449, 179.1479816184320271, -125.9940397287191161 ) ) ;
#8017 = DIRECTION ( 'NONE',  ( 0.000000000000000000, 0.000000000000000000, 1.000000000000000000 ) ) ;
#8018 = ORIENTED_EDGE ( 'NONE', *, *, #8880, .F. ) ;
#8019 = CYLINDRICAL_SURFACE ( 'NONE', #10000, 7.500000000000007105 ) ;
#8020 = CARTESIAN_POINT ( 'NONE',  ( -994.8066578865433485, 80.00401887192406036, -94.48732055948607922 ) ) ;
#8021 = CARTESIAN_POINT ( 'NONE',  ( -35.00000000000000000, 0.000000000000000000, 190.3192290001959464 ) ) ;
#8022 = CARTESIAN_POINT ( 'NONE',  ( -21.00772343926389141, 181.7109892249738436, -124.9456595701584831 ) ) ;
#8023 = CARTESIAN_POINT ( 'NONE',  ( 21.06267721941133786, 180.3886733041073001, -126.4187213689463505 ) ) ;
#8024 = CARTESIAN_POINT ( 'NONE',  ( 19.87738559348426648, 180.7004044570965675, -122.4687948322674345 ) ) ;
#8025 = CARTESIAN_POINT ( 'NONE',  ( -1010.947924043450712, 120.1731093567701407, -118.7903414690677408 ) ) ;
#8026 = CARTESIAN_POINT ( 'NONE',  ( -20.00000000000000000, 196.0000000000000000, -124.6807709998038405 ) ) ;
#8027 = FACE_BOUND ( 'NONE', #10846, .T. ) ;
#8028 = DIRECTION ( 'NONE',  ( 0.000000000000000000, 0.000000000000000000, 1.000000000000000000 ) ) ;
#8029 = MANIFOLD_SOLID_BREP ( 'Cut-Extrude4[1]', #2165 ) ;
#8030 = AXIS2_PLACEMENT_3D ( 'NONE', #8113, #11877, #3394 ) ;
#8031 =( REPRESENTATION_RELATIONSHIP ('NONE','NONE', #12149, #6140 ) REPRESENTATION_RELATIONSHIP_WITH_TRANSFORMATION ( #12109 )SHAPE_REPRESENTATION_RELATIONSHIP( ) );
#8032 = CYLINDRICAL_SURFACE ( 'NONE', #10260, 5.000000000000004441 ) ;
#8033 = CARTESIAN_POINT ( 'NONE',  ( -87.04832655144203102, 0.000000000000000000, -225.4289243767377116 ) ) ;
#8034 = ORIENTED_EDGE ( 'NONE', *, *, #8870, .F. ) ;
#8035 = CARTESIAN_POINT ( 'NONE',  ( -151.3258811035894098, 0.000000000000000000, -48.63263083939678921 ) ) ;
#8036 = CARTESIAN_POINT ( 'NONE',  ( -904.2101318206000542, 125.2895275102983419, -126.6442663926292340 ) ) ;
#8037 = CARTESIAN_POINT ( 'NONE',  ( 4.808665244885994618E-14, -6.000000000000000000, 141.4213562373094817 ) ) ;
#8038 = CARTESIAN_POINT ( 'NONE',  ( 1.387778780781445676E-14, 163.9999999999999716, 126.4213562373094959 ) ) ;
#8039 = EDGE_CURVE ( 'NONE', #83, #10273, #422, .T. ) ;
#8040 = CARTESIAN_POINT ( 'NONE',  ( 30.00000000000000000, -492.9999999999998863, -30.00000000000000000 ) ) ;
#8041 = ADVANCED_FACE ( 'NONE', ( #10822 ), #6866, .T. ) ;
#8042 = EDGE_LOOP ( 'NONE', ( #10969, #2366 ) ) ;
#8043 = VECTOR ( 'NONE', #755, 1000.000000000000000 ) ;
#8044 = ORIENTED_EDGE ( 'NONE', *, *, #6177, .T. ) ;
#8045 = CARTESIAN_POINT ( 'NONE',  ( -384.5742507613888392, 76.39205230857155016, -143.9146518029666311 ) ) ;
#8046 = CARTESIAN_POINT ( 'NONE',  ( -371.7911309421997998, 102.9548155466288080, -142.7648159640167194 ) ) ;
#8047 = CARTESIAN_POINT ( 'NONE',  ( -9.588412962918679838E-16, -0.8794428697894410840, 8.999999999999998224 ) ) ;
#8048 = AXIS2_PLACEMENT_3D ( 'NONE', #8833, #5177, #10747 ) ;
#8049 = DIRECTION ( 'NONE',  ( 0.000000000000000000, 0.000000000000000000, -1.000000000000000000 ) ) ;
#8050 = VECTOR ( 'NONE', #2431, 999.9999999999998863 ) ;
#8051 = DIRECTION ( 'NONE',  ( 0.000000000000000000, 0.5359254506312245425, 0.8442653086356912695 ) ) ;
#8052 = ORIENTED_EDGE ( 'NONE', *, *, #2543, .T. ) ;
#8053 = CARTESIAN_POINT ( 'NONE',  ( -975.9242088207953429, 48.36955882740826240, -146.0307792196450407 ) ) ;
#8054 = VERTEX_POINT ( 'NONE', #2183 ) ;
#8055 = ADVANCED_FACE ( 'NONE', ( #11762 ), #1528, .T. ) ;
#8056 = CARTESIAN_POINT ( 'NONE',  ( 57.50000000000000000, 0.000000000000000000, 0.000000000000000000 ) ) ;
#8057 = EDGE_LOOP ( 'NONE', ( #3482, #10997, #6702, #6254 ) ) ;
#8058 = DIRECTION ( 'NONE',  ( -1.000000000000000000, 0.000000000000000000, 0.000000000000000000 ) ) ;
#8059 = ORIENTED_EDGE ( 'NONE', *, *, #10020, .F. ) ;
#8060 = DIRECTION ( 'NONE',  ( -1.186840563529527301E-16, 1.000000000000000000, -0.000000000000000000 ) ) ;
#8061 = CIRCLE ( 'NONE', #2734, 7.500000000000007994 ) ;
#8062 = ORIENTED_EDGE ( 'NONE', *, *, #7730, .F. ) ;
#8063 = CIRCLE ( 'NONE', #2736, 7.500000000000007994 ) ;
#8064 = CARTESIAN_POINT ( 'NONE',  ( 30.00000000000000000, -492.9999999999998863, 30.00000000000000000 ) ) ;
#8065 = FACE_OUTER_BOUND ( 'NONE', #11942, .T. ) ;
#8066 = EDGE_CURVE ( 'NONE', #9472, #7241, #11643, .T. ) ;
#8067 = AXIS2_PLACEMENT_3D ( 'NONE', #6126, #9893, #372 ) ;
#8068 = CARTESIAN_POINT ( 'NONE',  ( -1037.550865396562358, 105.7975851359348241, -103.3307627799636350 ) ) ;
#8069 = DIRECTION ( 'NONE',  ( -0.000000000000000000, 1.000000000000000000, 0.000000000000000000 ) ) ;
#8070 = CIRCLE ( 'NONE', #8277, 7.500000000000007105 ) ;
#8071 = ORIENTED_EDGE ( 'NONE', *, *, #6747, .T. ) ;
#8072 = DIRECTION ( 'NONE',  ( 0.000000000000000000, -1.156482317317870246E-16, 1.000000000000000000 ) ) ;
#8073 = DIRECTION ( 'NONE',  ( 1.000000000000000000, 0.000000000000000000, 0.000000000000000000 ) ) ;
#8074 = VERTEX_POINT ( 'NONE', #7740 ) ;
#8075 = DIRECTION ( 'NONE',  ( 0.000000000000000000, 0.000000000000000000, -1.000000000000000000 ) ) ;
#8076 =( LENGTH_UNIT ( ) NAMED_UNIT ( * ) SI_UNIT ( .MILLI., .METRE. ) );
#8077 = DIRECTION ( 'NONE',  ( 0.000000000000000000, 0.000000000000000000, 1.000000000000000000 ) ) ;
#8078 = ORIENTED_EDGE ( 'NONE', *, *, #4663, .F. ) ;
#8079 = CARTESIAN_POINT ( 'NONE',  ( -828.6689926561751918, 79.96979452499502372, -154.4949334293652328 ) ) ;
#8080 = CARTESIAN_POINT ( 'NONE',  ( -1065.000000000006139, 76.10956187831460795, -95.06748246948023962 ) ) ;
#8081 = CARTESIAN_POINT ( 'NONE',  ( -262.5000000000000000, 139.9999999999999716, -126.4213562373076059 ) ) ;
#8082 = AXIS2_PLACEMENT_3D ( 'NONE', #12056, #1742, #6248 ) ;
#8083 = CLOSED_SHELL ( 'NONE', ( #9154, #1168, #5933, #3415, #1685, #7744, #7643, #1946, #5695, #9029, #4599, #3550, #1377, #4361 ) ) ;
#8084 = CARTESIAN_POINT ( 'NONE',  ( -1045.864486809339269, 115.5688325305735162, -126.6442663926293477 ) ) ;
#8085 = DIRECTION ( 'NONE',  ( 0.000000000000000000, -1.156482317317870246E-16, 1.000000000000000000 ) ) ;
#8086 = CARTESIAN_POINT ( 'NONE',  ( -1065.000000000008868, 109.8950841424299512, -113.1262384684097526 ) ) ;
#8087 = DIRECTION ( 'NONE',  ( -0.3117078928809153826, -1.979053562451413181E-14, -0.9501779778103363050 ) ) ;
#8088 = CIRCLE ( 'NONE', #2345, 7.500000000000007105 ) ;
#8089 = FACE_BOUND ( 'NONE', #10827, .T. ) ;
#8090 = CARTESIAN_POINT ( 'NONE',  ( -1063.013736978595261, 47.55218547899809067, -124.6807709998042242 ) ) ;
#8091 = CIRCLE ( 'NONE', #3747, 7.500000000000007105 ) ;
#8092 = VERTEX_POINT ( 'NONE', #3042 ) ;
#8093 = CYLINDRICAL_SURFACE ( 'NONE', #362, 7.500000000000007105 ) ;
#8094 = CARTESIAN_POINT ( 'NONE',  ( -1060.773655115450993, 112.4236047030758527, -118.7903414690679682 ) ) ;
#8095 = CARTESIAN_POINT ( 'NONE',  ( 6.899999999999999467, 10.39230484541326938, 0.000000000000000000 ) ) ;
#8096 = CARTESIAN_POINT ( 'NONE',  ( -240.0000000000000000, 139.9999999999999716, -126.4213562373078190 ) ) ;
#8097 = LINE ( 'NONE', #8154, #475 ) ;
#8098 = LINE ( 'NONE', #10933, #2807 ) ;
#8099 = ORIENTED_EDGE ( 'NONE', *, *, #9762, .F. ) ;
#8100 = CARTESIAN_POINT ( 'NONE',  ( -19.99524239788497226, 182.6919990222411343, -125.1313804517642581 ) ) ;
#8101 = DIRECTION ( 'NONE',  ( 0.000000000000000000, 0.000000000000000000, -1.000000000000000000 ) ) ;
#8102 = CARTESIAN_POINT ( 'NONE',  ( -1056.106496161729183, 78.18408418063155807, -154.8742214401234776 ) ) ;
#8103 = CARTESIAN_POINT ( 'NONE',  ( -826.3639150177631336, 74.35254223074741731, -143.1619793993637870 ) ) ;
#8104 = EDGE_CURVE ( 'NONE', #8014, #11084, #2510, .T. ) ;
#8105 = CARTESIAN_POINT ( 'NONE',  ( 0.5584673446549132114, -9.967293815311096594, 0.7361406979141401630 ) ) ;
#8106 = CARTESIAN_POINT ( 'NONE',  ( 7.653191805780027529E-16, 138.9999999999999716, -82.42135623730948168 ) ) ;
#8107 = CARTESIAN_POINT ( 'NONE',  ( 44.00000000000001421, 24.00000000000001776, -126.4213562373094959 ) ) ;
#8108 = EDGE_CURVE ( 'NONE', #2061, #5617, #5072, .T. ) ;
#8109 = CYLINDRICAL_SURFACE ( 'NONE', #12004, 7.499999999999978684 ) ;
#8110 = ORIENTED_EDGE ( 'NONE', *, *, #9929, .F. ) ;
#8111 = CARTESIAN_POINT ( 'NONE',  ( -1021.293373424891683, 59.24127555818969171, -141.4553492942756918 ) ) ;
#8112 = ORIENTED_EDGE ( 'NONE', *, *, #5465, .T. ) ;
#8113 = CARTESIAN_POINT ( 'NONE',  ( 126.4213562373094959, -494.9999999999998863, -6.938893903907228378E-15 ) ) ;
#8114 = FACE_BOUND ( 'NONE', #2244, .T. ) ;
#8115 = CARTESIAN_POINT ( 'NONE',  ( -19.97651234637680417, 180.1670482320588178, -126.1620355637344346 ) ) ;
#8116 = DIRECTION ( 'NONE',  ( -0.000000000000000000, 1.000000000000000000, -0.000000000000000000 ) ) ;
#8117 = ORIENTED_EDGE ( 'NONE', *, *, #4276, .F. ) ;
#8118 = DIRECTION ( 'NONE',  ( 0.000000000000000000, 1.000000000000000000, 0.000000000000000000 ) ) ;
#8119 = LINE ( 'NONE', #7882, #4610 ) ;
#8120 = ORIENTED_EDGE ( 'NONE', *, *, #10896, .F. ) ;
#8121 = AXIS2_PLACEMENT_3D ( 'NONE', #6329, #9301, #10967 ) ;
#8122 = DIRECTION ( 'NONE',  ( -1.000000000000000000, -1.186840563529527301E-16, 0.000000000000000000 ) ) ;
#8123 = EDGE_LOOP ( 'NONE', ( #2905, #6801 ) ) ;
#8124 = ADVANCED_FACE ( 'NONE', ( #6069 ), #9834, .F. ) ;
#8125 = DIRECTION ( 'NONE',  ( 0.000000000000000000, 0.000000000000000000, 1.000000000000000000 ) ) ;
#8126 = AXIS2_PLACEMENT_3D ( 'NONE', #4087, #6864, #6055 ) ;
#8127 = DIRECTION ( 'NONE',  ( -0.000000000000000000, -1.000000000000000000, -0.000000000000000000 ) ) ;
#8128 = CARTESIAN_POINT ( 'NONE',  ( -820.4595805503671500, 72.64106675864344709, -94.48732055948583763 ) ) ;
#8129 = LINE ( 'NONE', #6271, #11601 ) ;
#8130 = AXIS2_PLACEMENT_3D ( 'NONE', #413, #1481, #9008 ) ;
#8131 = VERTEX_POINT ( 'NONE', #6368 ) ;
#8132 = CYLINDRICAL_SURFACE ( 'NONE', #3628, 7.500000000000007105 ) ;
#8133 = DIRECTION ( 'NONE',  ( 1.000000000000000000, 0.000000000000000000, 0.000000000000000000 ) ) ;
#8134 = VERTEX_POINT ( 'NONE', #10948 ) ;
#8135 = ADVANCED_FACE ( 'NONE', ( #5249 ), #7240, .F. ) ;
#8136 = CARTESIAN_POINT ( 'NONE',  ( -853.6888141844383426, 53.84495383942796565, -96.78565065507952170 ) ) ;
#8137 = EDGE_CURVE ( 'NONE', #2477, #6316, #4279, .T. ) ;
#8138 = DIRECTION ( 'NONE',  ( 0.000000000000000000, -0.5273567215051647716, -0.8496439773713011512 ) ) ;
#8139 = DIRECTION ( 'NONE',  ( -1.000000000000000000, -3.061276722312011504E-17, 0.000000000000000000 ) ) ;
#8140 = CARTESIAN_POINT ( 'NONE',  ( -852.8175266017511831, 121.6828083272127685, -124.6807709998041247 ) ) ;
#8141 = VECTOR ( 'NONE', #6945, 999.9999999999998863 ) ;
#8142 = CARTESIAN_POINT ( 'NONE',  ( 35.00000000000000000, 81.99999999999998579, 190.3192290001959748 ) ) ;
#8143 = DIRECTION ( 'NONE',  ( 0.000000000000000000, 0.000000000000000000, -1.000000000000000000 ) ) ;
#8144 = FACE_BOUND ( 'NONE', #10995, .T. ) ;
#8145 = CARTESIAN_POINT ( 'NONE',  ( 0.000000000000000000, 0.000000000000000000, -89.68077099980401101 ) ) ;
#8146 = DIRECTION ( 'NONE',  ( -0.000000000000000000, -0.000000000000000000, -1.000000000000000000 ) ) ;
#8147 = MANIFOLD_SOLID_BREP ( 'Boss-Extrude8', #8295 ) ;
#8148 = ORIENTED_EDGE ( 'NONE', *, *, #3877, .T. ) ;
#8149 = DIRECTION ( 'NONE',  ( 0.000000000000000000, 0.000000000000000000, 1.000000000000000000 ) ) ;
#8150 = CIRCLE ( 'NONE', #2230, 5.999999999999999112 ) ;
#8151 = CARTESIAN_POINT ( 'NONE',  ( -926.5138833012644000, 125.7648744980332225, -122.7172756069789159 ) ) ;
#8152 = CARTESIAN_POINT ( 'NONE',  ( -35.00000000000000000, 81.99999999999998579, 260.3192290001960032 ) ) ;
#8153 = DIRECTION ( 'NONE',  ( -0.000000000000000000, -1.000000000000000000, -0.000000000000000000 ) ) ;
#8154 = CARTESIAN_POINT ( 'NONE',  ( -202.4999999999999716, -9.213203435596478030, -126.4213562373080180 ) ) ;
#8155 = CARTESIAN_POINT ( 'NONE',  ( 20.77152989773915692, 180.9696350864299461, -123.5256872951201217 ) ) ;
#8156 = EDGE_LOOP ( 'NONE', ( #687, #9011 ) ) ;
#8157 = CIRCLE ( 'NONE', #9541, 5.000000000000115463 ) ;
#8158 = ORIENTED_EDGE ( 'NONE', *, *, #903, .T. ) ;
#8159 = CARTESIAN_POINT ( 'NONE',  ( 20.77152989774015168, 180.9696350864370231, -123.5256872951244986 ) ) ;
#8160 = DIRECTION ( 'NONE',  ( -8.163404592832030268E-17, 1.000000000000000000, -0.000000000000000000 ) ) ;
#8161 = DIRECTION ( 'NONE',  ( 0.000000000000000000, -0.000000000000000000, 1.000000000000000000 ) ) ;
#8162 = CARTESIAN_POINT ( 'NONE',  ( -1031.794838716557251, 81.34535957697963227, -154.8742214401231649 ) ) ;
#8163 = CARTESIAN_POINT ( 'NONE',  ( 9.371890508914830252E-13, 152.0000000000000000, -36.42135623730948168 ) ) ;
#8164 = LINE ( 'NONE', #7302, #11537 ) ;
#8165 = DIRECTION ( 'NONE',  ( 0.000000000000000000, -1.156482317317870246E-16, 1.000000000000000000 ) ) ;
#8166 = VERTEX_POINT ( 'NONE', #6129 ) ;
#8167 = DIRECTION ( 'NONE',  ( 0.000000000000000000, 1.000000000000000000, 0.000000000000000000 ) ) ;
#8168 = AXIS2_PLACEMENT_3D ( 'NONE', #9739, #7833, #7898 ) ;
#8169 =( NAMED_UNIT ( * ) PLANE_ANGLE_UNIT ( ) SI_UNIT ( $, .RADIAN. ) );
#8170 = EDGE_LOOP ( 'NONE', ( #145, #3752, #4050, #11551 ) ) ;
#8171 = CARTESIAN_POINT ( 'NONE',  ( -1032.503061859593117, 50.81309391744441228, -141.4553492942758908 ) ) ;
#8172 = VERTEX_POINT ( 'NONE', #11071 ) ;
#8173 = ADVANCED_FACE ( 'NONE', ( #7113 ), #8109, .F. ) ;
#8174 = ORIENTED_EDGE ( 'NONE', *, *, #1452, .T. ) ;
#8175 = CIRCLE ( 'NONE', #6399, 7.500000000000007105 ) ;
#8176 = DIRECTION ( 'NONE',  ( 0.000000000000000000, 0.000000000000000000, 1.000000000000000000 ) ) ;
#8177 = ORIENTED_EDGE ( 'NONE', *, *, #2368, .F. ) ;
#8178 = CARTESIAN_POINT ( 'NONE',  ( -369.9377146894910311, 55.86387605661327171, -127.6416088482251467 ) ) ;
#8179 = LINE ( 'NONE', #7252, #427 ) ;
#8180 = ORIENTED_EDGE ( 'NONE', *, *, #6565, .T. ) ;
#8181 = CARTESIAN_POINT ( 'NONE',  ( 7.500000000000019540, 24.00000000000001421, -126.4213562373094959 ) ) ;
#8182 = ORIENTED_EDGE ( 'NONE', *, *, #8722, .T. ) ;
#8183 = CARTESIAN_POINT ( 'NONE',  ( -901.8785362142589292, 56.55314031071017666, -126.6442663926291061 ) ) ;
#8184 = VECTOR ( 'NONE', #4453, 1000.000000000000000 ) ;
#8185 = CIRCLE ( 'NONE', #2865, 7.500000000000013323 ) ;
#8186 = AXIS2_PLACEMENT_3D ( 'NONE', #11952, #2425, #7011 ) ;
#8187 = CYLINDRICAL_SURFACE ( 'NONE', #7007, 7.500000000000007105 ) ;
#8188 = CARTESIAN_POINT ( 'NONE',  ( -21.06240745282759974, 180.0655816779955956, -126.4269926335278882 ) ) ;
#8189 = CARTESIAN_POINT ( 'NONE',  ( 20.86817559351791473, 181.4710734879092797, -123.9731132673169185 ) ) ;
#8190 = EDGE_CURVE ( 'NONE', #5632, #505, #552, .T. ) ;
#8191 = DIRECTION ( 'NONE',  ( -0.000000000000000000, -1.000000000000000000, -0.000000000000000000 ) ) ;
#8192 = CARTESIAN_POINT ( 'NONE',  ( 6.247927005943220505E-13, 0.000000000000000000, -66.42135623730949590 ) ) ;
#8193 = EDGE_CURVE ( 'NONE', #7665, #8550, #7475, .T. ) ;
#8194 = MANIFOLD_SOLID_BREP ( 'Cut-Extrude5', #1181 ) ;
#8195 = CARTESIAN_POINT ( 'NONE',  ( -1020.082665824770629, 80.34198733739781062, -95.06748246948050962 ) ) ;
#8196 = CARTESIAN_POINT ( 'NONE',  ( -827.8285638327245124, 78.67432280806536937, -159.6807709998044800 ) ) ;
#8197 = DIRECTION ( 'NONE',  ( -1.000000000000000000, 0.000000000000000000, 0.000000000000000000 ) ) ;
#8198 = CIRCLE ( 'NONE', #2874, 7.500000000000007105 ) ;
#8199 = AXIS2_PLACEMENT_3D ( 'NONE', #6495, #4336, #11068 ) ;
#8200 = ORIENTED_EDGE ( 'NONE', *, *, #2583, .T. ) ;
#8201 = DIRECTION ( 'NONE',  ( -8.163404592832031500E-17, 1.000000000000000000, 0.000000000000000000 ) ) ;
#8202 = EDGE_CURVE ( 'NONE', #1855, #9681, #7264, .T. ) ;
#8203 = DIRECTION ( 'NONE',  ( 1.000000000000000000, 0.000000000000000000, 0.000000000000000000 ) ) ;
#8204 = ORIENTED_EDGE ( 'NONE', *, *, #3839, .T. ) ;
#8205 = CARTESIAN_POINT ( 'NONE',  ( -822.2219070778693322, 83.41200391691957350, -154.1554710663006347 ) ) ;
#8206 = CARTESIAN_POINT ( 'NONE',  ( -1013.120138696091999, 73.26074010992823560, -96.78565065507963538 ) ) ;
#8207 = DIRECTION ( 'NONE',  ( 0.000000000000000000, -0.000000000000000000, -1.000000000000000000 ) ) ;
#8208 = DIRECTION ( 'NONE',  ( -0.000000000000000000, -1.000000000000000000, -0.000000000000000000 ) ) ;
#8209 = CIRCLE ( 'NONE', #8604, 7.500000000000007105 ) ;
#8210 = CARTESIAN_POINT ( 'NONE',  ( 1.479627290717497352E-14, -6.000000000000000000, 118.9213562373094817 ) ) ;
#8211 = CARTESIAN_POINT ( 'NONE',  ( -19.89048104400029260, 179.2983987876859544, -122.5895104425266879 ) ) ;
#8212 = CARTESIAN_POINT ( 'NONE',  ( 1.249585401188644101E-12, -6.000000000000006217, 1.078643762690512986 ) ) ;
#8213 = EDGE_CURVE ( 'NONE', #8695, #11947, #560, .T. ) ;
#8214 = ORIENTED_EDGE ( 'NONE', *, *, #8496, .T. ) ;
#8215 = DIRECTION ( 'NONE',  ( -1.000000000000000000, -0.000000000000000000, -0.000000000000000000 ) ) ;
#8216 = CARTESIAN_POINT ( 'NONE',  ( -818.9561402410595292, 77.54029615563084121, -154.6639069421937904 ) ) ;
#8217 = AXIS2_PLACEMENT_3D ( 'NONE', #1772, #3480, #8460 ) ;
#8218 = ORIENTED_EDGE ( 'NONE', *, *, #6770, .F. ) ;
#8219 = DIRECTION ( 'NONE',  ( 1.000000000000000000, 0.000000000000000000, 0.000000000000000000 ) ) ;
#8220 = CARTESIAN_POINT ( 'NONE',  ( -1065.000000000006594, 112.0000000000007105, -124.6807709998041531 ) ) ;
#8221 = ADVANCED_FACE ( 'NONE', ( #11860 ), #12046, .F. ) ;
#8222 = CARTESIAN_POINT ( 'NONE',  ( -270.0000000000000000, -9.213203435596478030, -126.4213562373076059 ) ) ;
#8223 = CARTESIAN_POINT ( 'NONE',  ( -120.8820948793972434, 0.000000000000000000, -194.1989091883324363 ) ) ;
#8224 = CARTESIAN_POINT ( 'NONE',  ( -372.6850217215775274, 64.13912682578764191, -102.6824241675982989 ) ) ;
#8225 = CARTESIAN_POINT ( 'NONE',  ( 19.99143708932781749, 181.5311400647427149, -125.3935307427316701 ) ) ;
#8226 = EDGE_LOOP ( 'NONE', ( #6800, #11713 ) ) ;
#8227 = EDGE_LOOP ( 'NONE', ( #4043, #2623, #6297, #8963 ) ) ;
#8228 = AXIS2_PLACEMENT_3D ( 'NONE', #1533, #10188, #10121 ) ;
#8229 = EDGE_CURVE ( 'NONE', #11656, #11886, #1594, .T. ) ;
#8230 = CARTESIAN_POINT ( 'NONE',  ( -19.87204390493025130, 180.1031888591127768, -122.4220199087763064 ) ) ;
#8231 = LINE ( 'NONE', #10377, #8669 ) ;
#8232 = CARTESIAN_POINT ( 'NONE',  ( -1037.773541645230580, 93.34895244571352180, -152.5758913445289693 ) ) ;
#8233 = CARTESIAN_POINT ( 'NONE',  ( -824.1558762432750882, 73.68222816774749617, -142.8690915370046923 ) ) ;
#8234 = DIRECTION ( 'NONE',  ( 0.000000000000000000, 0.000000000000000000, 1.000000000000000000 ) ) ;
#8235 = DIRECTION ( 'NONE',  ( 1.000000000000000000, -1.262554838833776231E-16, 0.000000000000000000 ) ) ;
#8236 = CARTESIAN_POINT ( 'NONE',  ( -955.0423082396526979, 101.0797422464698769, -152.5758913445288272 ) ) ;
#8237 = CYLINDRICAL_SURFACE ( 'NONE', #1683, 7.500000000000007105 ) ;
#8238 = ORIENTED_EDGE ( 'NONE', *, *, #4594, .T. ) ;
#8239 = FACE_BOUND ( 'NONE', #5939, .T. ) ;
#8240 = ORIENTED_EDGE ( 'NONE', *, *, #8381, .T. ) ;
#8241 = CARTESIAN_POINT ( 'NONE',  ( 0.000000000000000000, -7.794228634059949812, -4.499999999999995559 ) ) ;
#8242 = CARTESIAN_POINT ( 'NONE',  ( -996.0013826475917540, 63.70094029248592449, -152.5758913445294240 ) ) ;
#8243 = AXIS2_PLACEMENT_3D ( 'NONE', #6466, #7517, #9435 ) ;
#8244 = B_SPLINE_CURVE_WITH_KNOTS ( 'NONE', 3,
 ( #713, #11845, #8016, #7265, #587, #7079, #6331, #6219, #6276, #11032, #3478, #4364, #3357, #3089 ),
 .UNSPECIFIED., .F., .F.,
 ( 4, 2, 2, 2, 2, 2, 4 ),
 ( 0.009574516480326976040, 0.01007331370637661733, 0.01057211093242625688, 0.01156970538452561578, 0.01256729983662497468, 0.01306609706267465414, 0.01356489428872433359 ),
 .UNSPECIFIED. ) ;
#8245 = VERTEX_POINT ( 'NONE', #605 ) ;
#8246 = CYLINDRICAL_SURFACE ( 'NONE', #7456, 7.500000000000020428 ) ;
#8247 = ORIENTED_EDGE ( 'NONE', *, *, #9069, .F. ) ;
#8248 = VECTOR ( 'NONE', #644, 1000.000000000000000 ) ;
#8249 = CARTESIAN_POINT ( 'NONE',  ( -372.5380659305778295, 62.41370632951886677, -128.7741405147628200 ) ) ;
#8250 = FACE_OUTER_BOUND ( 'NONE', #4660, .T. ) ;
#8251 = VERTEX_POINT ( 'NONE', #9132 ) ;
#8252 = ORIENTED_EDGE ( 'NONE', *, *, #580, .T. ) ;
#8253 = CARTESIAN_POINT ( 'NONE',  ( -823.8285638327243987, 78.67432280806571043, -264.6807709998050200 ) ) ;
#8254 = COLOUR_RGB ( '', 0.09019608, 0.27058824, 0.51372549) ;
#8255 = CARTESIAN_POINT ( 'NONE',  ( 0.1482032042127243432, 2.204400401860217240, 8.999999999999998224 ) ) ;
#8256 = CARTESIAN_POINT ( 'NONE',  ( 87.04832655144112152, 12.00000000000000000, -210.4289243767383368 ) ) ;
#8257 = CARTESIAN_POINT ( 'NONE',  ( -144.0488662551579182, 12.00000000000000000, -139.4077238332691877 ) ) ;
#8258 = CARTESIAN_POINT ( 'NONE',  ( -953.2897746444517679, 79.65961628290871488, -95.06748246948048120 ) ) ;
#8259 = DIRECTION ( 'NONE',  ( -1.000000000000000000, 0.000000000000000000, 0.000000000000000000 ) ) ;
#8260 = CARTESIAN_POINT ( 'NONE',  ( -828.8285638327206470, 78.67432280806529832, -144.4023295390027215 ) ) ;
#8261 = ADVANCED_BREP_SHAPE_REPRESENTATION ( '', ( #3942, #11957 ), #500 ) ;
#8262 = CARTESIAN_POINT ( 'NONE',  ( -375.0216849847562344, 81.99049224892637255, -94.61449237475785878 ) ) ;
#8263 = ORIENTED_EDGE ( 'NONE', *, *, #9793, .T. ) ;
#8264 = COLOUR_RGB ( '', 0.31764706, 0.68627451, 0.89019608) ;
#8265 = PLANE ( 'NONE',  #892 ) ;
#8266 = EDGE_CURVE ( 'NONE', #9384, #2064, #4511, .T. ) ;
#8267 = DIRECTION ( 'NONE',  ( 0.000000000000000000, 0.000000000000000000, 1.000000000000000000 ) ) ;
#8268 = ORIENTED_EDGE ( 'NONE', *, *, #7069, .F. ) ;
#8269 = CARTESIAN_POINT ( 'NONE',  ( -825.4463966093486533, 83.41668980410091194, -154.1315809916505088 ) ) ;
#8271 = EDGE_CURVE ( 'NONE', #7504, #4601, #1165, .T. ) ;
#8270 = CARTESIAN_POINT ( 'NONE',  ( -927.6556653799030983, 86.18751778479037284, -95.06748246948041015 ) ) ;
#8272 = DIRECTION ( 'NONE',  ( -0.000000000000000000, -1.000000000000000000, -0.000000000000000000 ) ) ;
#8273 = CYLINDRICAL_SURFACE ( 'NONE', #4869, 20.00000000000017053 ) ;
#8274 = CARTESIAN_POINT ( 'NONE',  ( 20.71964524312787148, 180.3384025927469736, -123.3053720114607614 ) ) ;
#8275 = DIRECTION ( 'NONE',  ( 3.061276722312011504E-17, -1.000000000000000000, 0.000000000000000000 ) ) ;
#8276 = VECTOR ( 'NONE', #5840, 1000.000000000000000 ) ;
#8277 = AXIS2_PLACEMENT_3D ( 'NONE', #3273, #9021, #7928 ) ;
#8278 = EDGE_CURVE ( 'NONE', #6648, #10083, #2147, .T. ) ;
#8279 = DIRECTION ( 'NONE',  ( 0.000000000000000000, 1.000000000000000000, 0.000000000000000000 ) ) ;
#8280 = DIRECTION ( 'NONE',  ( 0.000000000000000000, 0.000000000000000000, 1.000000000000000000 ) ) ;
#8281 = VERTEX_POINT ( 'NONE', #1420 ) ;
#8282 = DIRECTION ( 'NONE',  ( 0.000000000000000000, 0.000000000000000000, 1.000000000000000000 ) ) ;
#8283 = DIRECTION ( 'NONE',  ( -0.7071067811865477948, 0.000000000000000000, -0.7071067811865473507 ) ) ;
#8284 = AXIS2_PLACEMENT_3D ( 'NONE', #7156, #4262, #8028 ) ;
#8285 = ORIENTED_EDGE ( 'NONE', *, *, #5684, .F. ) ;
#8286 = CARTESIAN_POINT ( 'NONE',  ( 44.00000000000001421, 25.00000000000002132, -126.4213562373094959 ) ) ;
#8287 = CARTESIAN_POINT ( 'NONE',  ( -1010.947924043450712, 120.1731093567701407, -118.7903414690677408 ) ) ;
#8288 = DIRECTION ( 'NONE',  ( 0.000000000000000000, 0.000000000000000000, 1.000000000000000000 ) ) ;
#8289 = CARTESIAN_POINT ( 'NONE',  ( -154.5043356068770493, 12.00000000000000000, -102.0666613060160302 ) ) ;
#8290 = CYLINDRICAL_SURFACE ( 'NONE', #3640, 7.500000000000020428 ) ;
#8291 = ADVANCED_FACE ( 'NONE', ( #670 ), #3374, .F. ) ;
#8292 = CARTESIAN_POINT ( 'NONE',  ( 19.93132511079140556, 182.1895273313274117, -126.3410201175955478 ) ) ;
#8293 = VERTEX_POINT ( 'NONE', #9198 ) ;
#8294 = PRESENTATION_LAYER_ASSIGNMENT (  '', '', ( #3324 ) ) ;
#8295 = CLOSED_SHELL ( 'NONE', ( #4952, #5307, #9692, #11010, #3393, #3437, #4866, #7143, #5156, #5488, #3754, #2138, #7350, #9192 ) ) ;
#8296 = ORIENTED_EDGE ( 'NONE', *, *, #7087, .F. ) ;
#8297 = LINE ( 'NONE', #5499, #9856 ) ;
#8298 = CYLINDRICAL_SURFACE ( 'NONE', #10351, 7.500000000000007105 ) ;
#8299 = CARTESIAN_POINT ( 'NONE',  ( -1055.469533842436022, 91.91071092603651493, -152.5758913445291398 ) ) ;
#8300 = CARTESIAN_POINT ( 'NONE',  ( -823.1581254408829409, 73.70809864670252409, -142.8810402703306863 ) ) ;
#8301 = CARTESIAN_POINT ( 'NONE',  ( 0.07661102881317642666, 8.673996836102549679, -2.976196775178694853 ) ) ;
#8302 = PLANE ( 'NONE',  #6004 ) ;
#8303 = CARTESIAN_POINT ( 'NONE',  ( -1026.284439350006778, 91.37828661775253636, -154.2940595301281803 ) ) ;
#8304 = LINE ( 'NONE', #6307, #3250 ) ;
#8305 = ORIENTED_EDGE ( 'NONE', *, *, #1686, .F. ) ;
#8306 = CARTESIAN_POINT ( 'NONE',  ( 35.00000000000000000, 11.99999999999999289, 81.78351099501843180 ) ) ;
#8307 = VERTEX_POINT ( 'NONE', #8223 ) ;
#8308 = CARTESIAN_POINT ( 'NONE',  ( 0.8038475772933637575, -10.39230484541326405, -2.038422702671202938E-16 ) ) ;
#8309 = CARTESIAN_POINT ( 'NONE',  ( -1027.019426772554198, 78.04595964998465263, -154.2940595301285782 ) ) ;
#8310 = EDGE_CURVE ( 'NONE', #4288, #7231, #1538, .T. ) ;
#8311 = CARTESIAN_POINT ( 'NONE',  ( -20.72478464386518482, 180.4834696826887921, -123.3261552949825131 ) ) ;
#8312 = ORIENTED_EDGE ( 'NONE', *, *, #1495, .T. ) ;
#8313 = ORIENTED_EDGE ( 'NONE', *, *, #4645, .T. ) ;
#8314 = CARTESIAN_POINT ( 'NONE',  ( -19.90725264551396378, 181.9394096378942720, -126.6082001725200570 ) ) ;
#8315 = DIRECTION ( 'NONE',  ( 0.000000000000000000, 0.000000000000000000, -1.000000000000000000 ) ) ;
#8316 = CARTESIAN_POINT ( 'NONE',  ( -795.0000000000039790, 54.10491585757074517, -136.2353035311982410 ) ) ;
#8317 = VERTEX_POINT ( 'NONE', #3321 ) ;
#8318 = CARTESIAN_POINT ( 'NONE',  ( -379.2603478177108514, 62.16253007075349046, -127.3105118702911938 ) ) ;
#8319 = CARTESIAN_POINT ( 'NONE',  ( -19.00000000000000000, 196.0000000000000000, -124.6807709998038405 ) ) ;
#8320 = ORIENTED_EDGE ( 'NONE', *, *, #235, .T. ) ;
#8321 = CARTESIAN_POINT ( 'NONE',  ( -305.0000000000000568, 11.99999999999998224, -89.68077099980384048 ) ) ;
#8322 = FACE_OUTER_BOUND ( 'NONE', #2384, .T. ) ;
#8323 = FACE_OUTER_BOUND ( 'NONE', #7380, .T. ) ;
#8324 = CARTESIAN_POINT ( 'NONE',  ( -1065.000000000001364, 70.44548139156162847, -96.78565065507940801 ) ) ;
#8325 = DIRECTION ( 'NONE',  ( -0.000000000000000000, -1.000000000000000000, -1.757987137413040192E-14 ) ) ;
#8326 = PLANE ( 'NONE',  #1811 ) ;
#8327 = CARTESIAN_POINT ( 'NONE',  ( -1017.158871447983074, 53.64146012065780411, -126.6442663926291061 ) ) ;
#8328 = CARTESIAN_POINT ( 'NONE',  ( -820.5266942580660725, 82.43260598963610164, -144.6763645173222130 ) ) ;
#8329 = ORIENTED_EDGE ( 'NONE', *, *, #253, .F. ) ;
#8330 = CARTESIAN_POINT ( 'NONE',  ( -825.1286147475018424, 83.51336106040476182, -144.6235354408670162 ) ) ;
#8331 = DIRECTION ( 'NONE',  ( 0.9997638558560747457, 1.186560298089790222E-16, -0.02173091171106836944 ) ) ;
#8332 =( LENGTH_UNIT ( ) NAMED_UNIT ( * ) SI_UNIT ( .MILLI., .METRE. ) );
#8333 = VERTEX_POINT ( 'NONE', #11919 ) ;
#8334 = CARTESIAN_POINT ( 'NONE',  ( -996.5513353153756952, 56.29506814688433280, -99.57582448894517313 ) ) ;
#8335 = DIRECTION ( 'NONE',  ( 0.000000000000000000, 1.000000000000000000, -0.000000000000000000 ) ) ;
#8336 = CARTESIAN_POINT ( 'NONE',  ( 2.510525938252073693E-14, -7.999999999999979572, -124.6807709998038405 ) ) ;
#8337 = AXIS2_PLACEMENT_3D ( 'NONE', #1767, #7328, #4615 ) ;
#8338 = EDGE_CURVE ( 'NONE', #4125, #7035, #7164, .T. ) ;
#8339 = CARTESIAN_POINT ( 'NONE',  ( -820.5035528205692117, 74.92619343081587147, -105.9719278460591596 ) ) ;
#8340 = CARTESIAN_POINT ( 'NONE',  ( -19.87629508054677174, 179.7764057819409516, -122.4594234116466538 ) ) ;
#8341 = CARTESIAN_POINT ( 'NONE',  ( -821.7324155770269272, 74.13196894618555177, -143.0682369473086055 ) ) ;
#8342 = ORIENTED_EDGE ( 'NONE', *, *, #10225, .F. ) ;
#8343 = ORIENTED_EDGE ( 'NONE', *, *, #1101, .T. ) ;
#8344 = CARTESIAN_POINT ( 'NONE',  ( -369.9928909712432983, 56.00132045696368976, -120.5003237462438221 ) ) ;
#8345 = ITEM_DEFINED_TRANSFORMATION ( 'NONE', 'NONE', #12178,  #11957 ) ;
#8346 = CARTESIAN_POINT ( 'NONE',  ( -381.0253547164383008, 98.60296799592514105, -113.5251504039077588 ) ) ;
#8347 = ORIENTED_EDGE ( 'NONE', *, *, #4178, .T. ) ;
#8348 = CARTESIAN_POINT ( 'NONE',  ( 6.899999999999999467, 0.000000000000000000, 8.999999999999998224 ) ) ;
#8349 = DIRECTION ( 'NONE',  ( -1.000000000000000000, 0.000000000000000000, 0.000000000000000000 ) ) ;
#8350 = CARTESIAN_POINT ( 'NONE',  ( 20.00000000000000355, 177.7115707886026144, -124.6807709998038547 ) ) ;
#8351 = CYLINDRICAL_SURFACE ( 'NONE', #9381, 57.99999999999999289 ) ;
#8352 = AXIS2_PLACEMENT_3D ( 'NONE', #6122, #11689, #3322 ) ;
#8353 = CARTESIAN_POINT ( 'NONE',  ( 19.96746008154850927, 182.3013212999341590, -123.5332635133612200 ) ) ;
#8354 = EDGE_LOOP ( 'NONE', ( #3032, #5825 ) ) ;
#8355 = ORIENTED_EDGE ( 'NONE', *, *, #6062, .F. ) ;
#8356 = EDGE_CURVE ( 'NONE', #9220, #2139, #9036, .T. ) ;
#8357 = CARTESIAN_POINT ( 'NONE',  ( -795.0000000000043201, 102.0000000000005684, -124.6807709998040963 ) ) ;
#8358 = CARTESIAN_POINT ( 'NONE',  ( 21.06240745282767435, 180.2041921146315246, -126.4269926335259413 ) ) ;
#8359 = CARTESIAN_POINT ( 'NONE',  ( -927.2951026182241776, 99.13268410970675859, -154.2940595301278961 ) ) ;
#8360 = CARTESIAN_POINT ( 'NONE',  ( -372.4203662516890745, 101.9987822128686048, -123.8978246257192097 ) ) ;
#8361 = CIRCLE ( 'NONE', #1241, 7.500000000000007105 ) ;
#8362 =( BOUNDED_SURFACE ( )  B_SPLINE_SURFACE ( 3, 2, ( 
 ( #773, #6390, #3791 ),
 ( #3532, #7325, #2809 ),
 ( #11156, #11090, #6454 ),
 ( #12154, #10162, #1695 ),
 ( #2682, #10227, #7564 ),
 ( #9233, #3669, #4547 ),
 ( #2749, #6519, #5587 ),
 ( #10286, #1826, #909 ),
 ( #4841, #3856, #8685 ),
 ( #3050, #78, #2129 ),
 ( #5888, #8738, #255 ),
 ( #4046, #10829, #6317 ),
 ( #6075, #9842, #2367 ),
 ( #10884, #6135, #1378 ),
 ( #5141, #2482, #11142 ),
 ( #3901, #7863, #1006 ),
 ( #6802, #9650, #2049 ),
 ( #5693, #6927, #4775 ),
 ( #6870, #11445, #3841 ),
 ( #10638, #126, #9711 ),
 ( #11383, #6683, #1993 ),
 ( #5751, #1071, #8951 ),
 ( #7170, #416, #11809 ),
 ( #10011, #3326, #10936 ),
 ( #10868, #2467, #6243 ),
 ( #4205, #5240, #7981 ),
 ( #5998, #11752, #2404 ),
 ( #9075, #9012, #9766 ),
 ( #610, #547, #3447 ),
 ( #4386, #1310, #8159 ) ),
 .UNSPECIFIED., .F., .F., .F. ) 
 B_SPLINE_SURFACE_WITH_KNOTS ( ( 4, 2, 2, 2, 2, 2, 2, 2, 2, 2, 2, 2, 2, 2, 4 ),
 ( 3, 3 ),
 ( 0.000000000000000000, 0.0004931090571482092720, 0.0009862181142964185441, 0.001479327171444627925, 0.001972436228592837088, 0.002958654342889255849, 0.003451763400037465013, 0.003944872457185674176, 0.004437981514333883340, 0.004931090571482093371, 0.005424199628630302535, 0.005917308685778511698, 0.006410417742926720862, 0.006903526800074930025, 0.007889744914371348353 ),
 ( 0.000000000000000000, 1.000000000000000000 ),
 .UNSPECIFIED. ) 
 GEOMETRIC_REPRESENTATION_ITEM ( )  RATIONAL_B_SPLINE_SURFACE ( (
 ( 1.000000000000000000, 0.6687969305523246977, 1.000000000000000000),
 ( 1.000000000000000000, 0.6694841494169265772, 1.000000000000000000),
 ( 1.000000000000000000, 0.6703808696174045068, 1.000000000000000000),
 ( 1.000000000000000000, 0.6727883736869240128, 1.000000000000000000),
 ( 1.000000000000000000, 0.6743212217357245075, 1.000000000000000000),
 ( 1.000000000000000000, 0.6781193367449044329, 1.000000000000000000),
 ( 1.000000000000000000, 0.6803721377959787153, 1.000000000000000000),
 ( 1.000000000000000000, 0.6857220711556456516, 1.000000000000000000),
 ( 1.000000000000000000, 0.6888414615222259174, 1.000000000000000000),
 ( 1.000000000000000000, 0.6991960670388784882, 1.000000000000000000),
 ( 1.000000000000000000, 0.7077353972677926652, 1.000000000000000000),
 ( 1.000000000000000000, 0.7216195274859381614, 1.000000000000000000),
 ( 1.000000000000000000, 0.7264787526967504405, 1.000000000000000000),
 ( 1.000000000000000000, 0.7363107972878868424, 1.000000000000000000),
 ( 1.000000000000000000, 0.7412133880338421799, 1.000000000000000000),
 ( 1.000000000000000000, 0.7508641489171165029, 1.000000000000000000),
 ( 1.000000000000000000, 0.7556596050786191787, 1.000000000000000000),
 ( 1.000000000000000000, 0.7646032520811554267, 1.000000000000000000),
 ( 1.000000000000000000, 0.7687769290552097790, 1.000000000000000000),
 ( 1.000000000000000000, 0.7763903678017805010, 1.000000000000000000),
 ( 1.000000000000000000, 0.7798239438996181772, 1.000000000000000000),
 ( 1.000000000000000000, 0.7855160016894544572, 1.000000000000000000),
 ( 1.000000000000000000, 0.7878236855009348449, 1.000000000000000000),
 ( 1.000000000000000000, 0.7912368103514670903, 1.000000000000000000),
 ( 1.000000000000000000, 0.7922947285227288639, 1.000000000000000000),
 ( 1.000000000000000000, 0.7930773382062819010, 1.000000000000000000),
 ( 1.000000000000000000, 0.7928003068872482295, 1.000000000000000000),
 ( 1.000000000000000000, 0.7899630766598022547, 1.000000000000000000),
 ( 1.000000000000000000, 0.7854601384747740278, 1.000000000000000000),
 ( 1.000000000000000000, 0.7788034628475056786, 1.000000000000000000) ) ) 
 REPRESENTATION_ITEM ( '' )  SURFACE ( )  );
#8363 = SURFACE_STYLE_USAGE ( .BOTH. , #4587 ) ;
#8364 = DIRECTION ( 'NONE',  ( 1.000000000000000000, 0.000000000000000000, 0.000000000000000000 ) ) ;
#8365 = FACE_OUTER_BOUND ( 'NONE', #9975, .T. ) ;
#8366 = VERTEX_POINT ( 'NONE', #3558 ) ;
#8367 = DIRECTION ( 'NONE',  ( 0.000000000000000000, 0.000000000000000000, -1.000000000000000000 ) ) ;
#8368 = CARTESIAN_POINT ( 'NONE',  ( -373.2167405728580434, 97.70338709260114740, -148.7255640766979354 ) ) ;
#8369 = VERTEX_POINT ( 'NONE', #7102 ) ;
#8370 = CARTESIAN_POINT ( 'NONE',  ( -794.9999999999992042, 76.10956187831466480, -154.2940595301278393 ) ) ;
#8371 = CARTESIAN_POINT ( 'NONE',  ( 19.86104407927658144, 181.3041390551380800, -127.0369522072293194 ) ) ;
#8372 = ORIENTED_EDGE ( 'NONE', *, *, #9069, .T. ) ;
#8373 = VERTEX_POINT ( 'NONE', #2399 ) ;
#8374 = CARTESIAN_POINT ( 'NONE',  ( -19.98868386570119782, 182.5424741720831889, -123.9930727067244902 ) ) ;
#8375 = EDGE_CURVE ( 'NONE', #8983, #9395, #7347, .T. ) ;
#8376 = CARTESIAN_POINT ( 'NONE',  ( -827.8143761345677376, 75.63828352384309994, -105.7174308425206419 ) ) ;
#8377 = CARTESIAN_POINT ( 'NONE',  ( -954.4431216459919369, 51.77564274757662588, -136.2353035311985820 ) ) ;
#8378 = ADVANCED_FACE ( 'NONE', ( #10124 ), #1657, .F. ) ;
#8379 = VECTOR ( 'NONE', #1779, 1000.000000000000000 ) ;
#8380 = VERTEX_POINT ( 'NONE', #9007 ) ;
#8381 = EDGE_CURVE ( 'NONE', #10282, #1185, #11120, .T. ) ;
#8382 = CARTESIAN_POINT ( 'NONE',  ( -382.0430766089316421, 67.63206925129327374, -138.5972335451334629 ) ) ;
#8383 = CARTESIAN_POINT ( 'NONE',  ( -35.00000000000000000, 81.99999999999998579, 190.3192290001959748 ) ) ;
#8384 = FACE_OUTER_BOUND ( 'NONE', #4666, .T. ) ;
#8385 = CARTESIAN_POINT ( 'NONE',  ( 154.5043356068769071, 12.00000000000000000, -94.56666130601712439 ) ) ;
#8386 = EDGE_CURVE ( 'NONE', #3022, #2997, #10004, .T. ) ;
#8387 = CARTESIAN_POINT ( 'NONE',  ( -35.00000000000000000, 81.99999999999998579, 190.3192290001959748 ) ) ;
#8388 = CIRCLE ( 'NONE', #2446, 7.500000000000005329 ) ;
#8389 = AXIS2_PLACEMENT_3D ( 'NONE', #10760, #420, #7987 ) ;
#8390 = DIRECTION ( 'NONE',  ( 0.000000000000000000, 1.000000000000000000, 0.000000000000000000 ) ) ;
#8391 = CARTESIAN_POINT ( 'NONE',  ( -89.99999999999998579, 12.00000000000001421, -126.4213562373088564 ) ) ;
#8392 = DIRECTION ( 'NONE',  ( -0.7071067811865473507, 0.000000000000000000, 0.7071067811865477948 ) ) ;
#8393 = EDGE_CURVE ( 'NONE', #11782, #1835, #11814, .T. ) ;
#8394 = ORIENTED_EDGE ( 'NONE', *, *, #8749, .F. ) ;
#8395 = CIRCLE ( 'NONE', #10545, 7.500000000000007105 ) ;
#8396 = CARTESIAN_POINT ( 'NONE',  ( -819.4849966174430165, 81.17290644373777297, -144.6655594550751402 ) ) ;
#8397 = CIRCLE ( 'NONE', #9760, 7.500000000000007105 ) ;
#8398 =( LENGTH_UNIT ( ) NAMED_UNIT ( * ) SI_UNIT ( .MILLI., .METRE. ) );
#8399 = AXIS2_PLACEMENT_3D ( 'NONE', #1038, #9615, #9098 ) ;
#8400 = CARTESIAN_POINT ( 'NONE',  ( -369.9107093661896215, 108.2030601565901549, -126.5620920014721094 ) ) ;
#8401 = ORIENTED_EDGE ( 'NONE', *, *, #4594, .F. ) ;
#8402 = CARTESIAN_POINT ( 'NONE',  ( -818.1708872189576596, 40.82851623284144438, -103.3307627799635640 ) ) ;
#8403 = CARTESIAN_POINT ( 'NONE',  ( -365.0000000000000568, 102.0000000000000142, -124.6807709998038405 ) ) ;
#8404 = CARTESIAN_POINT ( 'NONE',  ( -379.7921418149276747, 53.60747417478052057, -114.9924028573224035 ) ) ;
#8405 = DIRECTION ( 'NONE',  ( 1.000000000000000000, -1.262554838833776231E-16, 0.000000000000000000 ) ) ;
#8406 = CARTESIAN_POINT ( 'NONE',  ( -30.00000000000000000, -492.9999999999998863, 30.00000000000000000 ) ) ;
#8407 = AXIS2_PLACEMENT_3D ( 'NONE', #10391, #7554, #4776 ) ;
#8408 = CIRCLE ( 'NONE', #3863, 7.500000000000007994 ) ;
#8409 = CARTESIAN_POINT ( 'NONE',  ( -819.4847856676369702, 76.17713329584734083, -105.5450962460538165 ) ) ;
#8410 = CARTESIAN_POINT ( 'NONE',  ( -20.72447511889459904, 179.9475203146823787, -123.3250521315598718 ) ) ;
#8411 = CARTESIAN_POINT ( 'NONE',  ( -826.0729559276762757, 74.19411019796167750, -143.0951037527838139 ) ) ;
#8412 = ORIENTED_EDGE ( 'NONE', *, *, #7262, .F. ) ;
#8413 = CARTESIAN_POINT ( 'NONE',  ( -373.0692867644656872, 65.64952826050301837, -148.1814920571080734 ) ) ;
#8414 = ITEM_DEFINED_TRANSFORMATION ( 'NONE', 'NONE', #11193,  #11957 ) ;
#8415 = CARTESIAN_POINT ( 'NONE',  ( -383.1555409210616290, 93.38962432455592477, -108.2374382966716837 ) ) ;
#8416 = ORIENTED_EDGE ( 'NONE', *, *, #4786, .T. ) ;
#8417 = CARTESIAN_POINT ( 'NONE',  ( -1037.392967692957200, 114.2240391150264855, -113.1262384684098805 ) ) ;
#8418 = AXIS2_PLACEMENT_3D ( 'NONE', #9600, #9228, #10891 ) ;
#8419 = AXIS2_PLACEMENT_3D ( 'NONE', #10848, #4247, #8017 ) ;
#8420 = FACE_OUTER_BOUND ( 'NONE', #10727, .T. ) ;
#8421 = CARTESIAN_POINT ( 'NONE',  ( 19.99569434005708857, 181.6422274730699371, -125.1461840823352816 ) ) ;
#8422 = EDGE_LOOP ( 'NONE', ( #7811, #1770, #10400, #9545 ) ) ;
#8423 = DIRECTION ( 'NONE',  ( -8.163404592832030268E-17, 1.000000000000000000, -0.000000000000000000 ) ) ;
#8424 = CARTESIAN_POINT ( 'NONE',  ( -157.5000000000000000, -9.213203435596451385, -126.4213562373084301 ) ) ;
#8425 = CARTESIAN_POINT ( 'NONE',  ( -993.0619804577135028, 103.7129695969640579, -149.7857175106631757 ) ) ;
#8426 =( LENGTH_UNIT ( ) NAMED_UNIT ( * ) SI_UNIT ( .MILLI., .METRE. ) );
#8427 = CARTESIAN_POINT ( 'NONE',  ( -305.0000000000000568, 24.00000000000000711, -159.6807709998038547 ) ) ;
#8428 = CARTESIAN_POINT ( 'NONE',  ( -1023.463303304735746, 92.47874188371233117, -154.2940595301281519 ) ) ;
#8429 = EDGE_LOOP ( 'NONE', ( #4124, #11504, #12165, #11569 ) ) ;
#8430 = DIRECTION ( 'NONE',  ( 0.000000000000000000, 0.000000000000000000, 1.000000000000000000 ) ) ;
#8431 = EDGE_CURVE ( 'NONE', #8293, #4980, #9263, .T. ) ;
#8432 = PRODUCT_DEFINITION_SHAPE ( 'NONE', 'NONE',  #12251 ) ;
#8433 = VERTEX_POINT ( 'NONE', #1851 ) ;
#8434 = CARTESIAN_POINT ( 'NONE',  ( -952.9945178120615310, 87.05516224832936700, -154.8742214401229660 ) ) ;
#8435 = ADVANCED_FACE ( 'NONE', ( #12182 ), #11253, .F. ) ;
#8436 = VERTEX_POINT ( 'NONE', #3410 ) ;
#8437 = CARTESIAN_POINT ( 'NONE',  ( 19.94501782540249124, 182.3171294987543263, -126.1758857494099146 ) ) ;
#8438 = EDGE_LOOP ( 'NONE', ( #10314, #2304, #2541, #11772 ) ) ;
#8439 = AXIS2_PLACEMENT_3D ( 'NONE', #5826, #9603, #1019 ) ;
#8440 = VERTEX_POINT ( 'NONE', #9391 ) ;
#8441 = EDGE_CURVE ( 'NONE', #5632, #6035, #4250, .T. ) ;
#8442 = CARTESIAN_POINT ( 'NONE',  ( -151.3258811035894098, 12.00000000000000000, -48.63263083939678921 ) ) ;
#8443 = CARTESIAN_POINT ( 'NONE',  ( -21.03188327321321083, 181.6721105287138300, -125.2135271367785236 ) ) ;
#8444 = DIRECTION ( 'NONE',  ( 0.000000000000000000, 0.000000000000000000, 1.000000000000000000 ) ) ;
#8445 = CARTESIAN_POINT ( 'NONE',  ( -371.6769972486663960, 60.68164136501989248, -142.2120404103473561 ) ) ;
#8446 = DIRECTION ( 'NONE',  ( 0.000000000000000000, 0.000000000000000000, 1.000000000000000000 ) ) ;
#8447 = VECTOR ( 'NONE', #10369, 1000.000000000000000 ) ;
#8448 = APPLICATION_CONTEXT ( 'automotive_design' ) ;
#8449 = DIRECTION ( 'NONE',  ( 1.000000000000000000, 0.000000000000000000, -0.000000000000000000 ) ) ;
#8450 = ADVANCED_FACE ( 'NONE', ( #4754 ), #5735, .T. ) ;
#8451 = CARTESIAN_POINT ( 'NONE',  ( -1.248124223602892907E-14, -7.573738413550446857, 4.881900264494497321 ) ) ;
#8452 = CARTESIAN_POINT ( 'NONE',  ( -120.8820948793972434, 12.00000000000000000, -186.6989091883324363 ) ) ;
#8453 = AXIS2_PLACEMENT_3D ( 'NONE', #10043, #9173, #7260 ) ;
#8454 = CARTESIAN_POINT ( 'NONE',  ( -1065.000000000007049, 56.89504896194527106, -107.9061927053324581 ) ) ;
#8455 = CARTESIAN_POINT ( 'NONE',  ( -826.3398728605918677, 83.01019204304884624, -104.7054730589236016 ) ) ;
#8456 = CARTESIAN_POINT ( 'NONE',  ( -976.2517683711890868, 35.25052392388818134, -126.6442663926290777 ) ) ;
#8457 = CARTESIAN_POINT ( 'NONE',  ( -951.5459139781262365, 122.3346817490816676, -136.2353035311979852 ) ) ;
#8458 = ORIENTED_EDGE ( 'NONE', *, *, #3247, .F. ) ;
#8459 = CYLINDRICAL_SURFACE ( 'NONE', #7789, 7.500000000000007105 ) ;
#8460 = DIRECTION ( 'NONE',  ( 1.000000000000000000, 0.000000000000000000, 0.000000000000000000 ) ) ;
#8461 = ORIENTED_EDGE ( 'NONE', *, *, #9229, .T. ) ;
#8462 = CARTESIAN_POINT ( 'NONE',  ( -1013.637332661006667, 62.09754518945625534, -103.3307627799637913 ) ) ;
#8463 = AXIS2_PLACEMENT_3D ( 'NONE', #1371, #7178, #7365 ) ;
#8464 = CARTESIAN_POINT ( 'NONE',  ( -217.5000000000000000, -9.213203435596478030, -126.4213562373080180 ) ) ;
#8465 = CARTESIAN_POINT ( 'NONE',  ( 20.75549287943134402, 180.8556829965724546, -123.4547523536870557 ) ) ;
#8466 = CARTESIAN_POINT ( 'NONE',  ( 19.85548708303895893, 179.2177006722742192, -127.0812667107773564 ) ) ;
#8467 = EDGE_CURVE ( 'NONE', #10476, #1493, #8063, .T. ) ;
#8468 = CARTESIAN_POINT ( 'NONE',  ( -1018.154501869011938, 114.3413228342526082, -107.9061927053323870 ) ) ;
#8469 = CARTESIAN_POINT ( 'NONE',  ( 1.249585401188644101E-12, -6.000000000000005329, -6.421356237309495008 ) ) ;
#8470 = VECTOR ( 'NONE', #1478, 1000.000000000000000 ) ;
#8471 = ORIENTED_EDGE ( 'NONE', *, *, #7723, .T. ) ;
#8472 = CARTESIAN_POINT ( 'NONE',  ( -37.50000000000000711, 152.0000000000000000, -126.4213562373092685 ) ) ;
#8473 = CARTESIAN_POINT ( 'NONE',  ( -373.4274415647627166, 98.04483789281530903, -112.6589849898505236 ) ) ;
#8474 = ORIENTED_EDGE ( 'NONE', *, *, #11897, .F. ) ;
#8475 = CARTESIAN_POINT ( 'NONE',  ( -1065.000000000000455, 107.1049510380560719, -107.9061927053323302 ) ) ;
#8476 = AXIS2_PLACEMENT_3D ( 'NONE', #174, #7724, #11850 ) ;
#8477 = CARTESIAN_POINT ( 'NONE',  ( 0.000000000000000000, 1.102182119232617517E-15, -8.999999999999998224 ) ) ;
#8478 = VECTOR ( 'NONE', #11404, 1000.000000000000000 ) ;
#8479 = ORIENTED_EDGE ( 'NONE', *, *, #1932, .F. ) ;
#8480 = ORIENTED_EDGE ( 'NONE', *, *, #11375, .T. ) ;
#8481 = CIRCLE ( 'NONE', #3130, 35.00000000000000711 ) ;
#8482 = DIRECTION ( 'NONE',  ( -0.000000000000000000, 1.189524669241239115E-16, -1.000000000000000000 ) ) ;
#8483 = CARTESIAN_POINT ( 'NONE',  ( -30.00000000000000000, -492.9999999999998863, -30.00000000000000000 ) ) ;
#8484 = CARTESIAN_POINT ( 'NONE',  ( -974.9912860506709649, 88.33816101283774458, -154.2940595301278108 ) ) ;
#8485 = DIRECTION ( 'NONE',  ( 1.000000000000000000, 0.000000000000000000, 0.000000000000000000 ) ) ;
#8486 = DIRECTION ( 'NONE',  ( -1.000000000000000000, -0.000000000000000000, -0.000000000000000000 ) ) ;
#8487 = CARTESIAN_POINT ( 'NONE',  ( -1019.017691546887363, 99.44610047464912839, -152.5758913445291967 ) ) ;
#8488 = DIRECTION ( 'NONE',  ( -0.000000000000000000, 1.000000000000000000, -0.000000000000000000 ) ) ;
#8489 = ORIENTED_EDGE ( 'NONE', *, *, #4478, .T. ) ;
#8490 = ORIENTED_EDGE ( 'NONE', *, *, #4894, .F. ) ;
#8491 = CARTESIAN_POINT ( 'NONE',  ( -1023.860074334738101, 85.97273905232952984, -154.8742214401228523 ) ) ;
#8492 = PRESENTATION_LAYER_ASSIGNMENT (  '', '', ( #5300 ) ) ;
#8493 = AXIS2_PLACEMENT_3D ( 'NONE', #7965, #1524, #2339 ) ;
#8494 = ORIENTED_EDGE ( 'NONE', *, *, #3666, .F. ) ;
#8495 = ORIENTED_EDGE ( 'NONE', *, *, #5979, .F. ) ;
#8496 = EDGE_CURVE ( 'NONE', #11020, #11584, #3760, .T. ) ;
#8497 = CARTESIAN_POINT ( 'NONE',  ( -19.94556339419311186, 182.0394078756253293, -123.1838850670707188 ) ) ;
#8498 = DIRECTION ( 'NONE',  ( -1.000000000000000000, 0.000000000000000000, 0.000000000000000000 ) ) ;
#8499 = EDGE_LOOP ( 'NONE', ( #9501, #4410, #4805 ) ) ;
#8500 = CARTESIAN_POINT ( 'NONE',  ( -374.4362727378983777, 73.12462464385868088, -152.9182541025093940 ) ) ;
#8501 = DIRECTION ( 'NONE',  ( 1.000000000000000000, 0.000000000000000000, -0.000000000000000000 ) ) ;
#8502 = CARTESIAN_POINT ( 'NONE',  ( -374.8916234221949821, 78.08292650439227600, -95.01254429865261386 ) ) ;
#8503 = CYLINDRICAL_SURFACE ( 'NONE', #3907, 7.500000000000007105 ) ;
#8504 = DIRECTION ( 'NONE',  ( 0.000000000000000000, 0.000000000000000000, 1.000000000000000000 ) ) ;
#8505 = LINE ( 'NONE', #5525, #1450 ) ;
#8506 = CARTESIAN_POINT ( 'NONE',  ( -1016.402231264574652, 68.39482517277133411, -99.57582448894554261 ) ) ;
#8507 = CARTESIAN_POINT ( 'NONE',  ( -823.1752771847307031, 83.64233931405222222, -104.7482132693511403 ) ) ;
#8508 = EDGE_CURVE ( 'NONE', #8781, #6173, #10435, .T. ) ;
#8509 = EDGE_CURVE ( 'NONE', #9164, #11519, #3916, .T. ) ;
#8510 = ORIENTED_EDGE ( 'NONE', *, *, #11988, .T. ) ;
#8511 = CARTESIAN_POINT ( 'NONE',  ( -828.6712641482251911, 79.96111424986069949, -144.5792126457444908 ) ) ;
#8512 = ADVANCED_FACE ( 'NONE', ( #8420 ), #4812, .F. ) ;
#8513 = DIRECTION ( 'NONE',  ( 3.061276722312011504E-17, -1.000000000000000000, -0.000000000000000000 ) ) ;
#8514 = ORIENTED_EDGE ( 'NONE', *, *, #9932, .F. ) ;
#8515 = CARTESIAN_POINT ( 'NONE',  ( -1032.503061859599256, 50.81309391744463255, -107.9061927053326428 ) ) ;
#8516 = DIRECTION ( 'NONE',  ( 0.000000000000000000, 1.000000000000000000, 0.000000000000000000 ) ) ;
#8517 = AXIS2_PLACEMENT_3D ( 'NONE', #5394, #1829, #8197 ) ;
#8518 = CARTESIAN_POINT ( 'NONE',  ( -1011.051362836439694, 118.1813008219151868, -113.1262384684097952 ) ) ;
#8519 = CARTESIAN_POINT ( 'NONE',  ( -150.0000000000000000, 24.00000000000001421, -126.4213562373084301 ) ) ;
#8520 = EDGE_LOOP ( 'NONE', ( #11581, #10010 ) ) ;
#8521 = PRODUCT_DEFINITION_SHAPE ( 'NONE', 'NONE',  #1872 ) ;
#8522 = CARTESIAN_POINT ( 'NONE',  ( -374.2864773846411595, 92.10316615029381637, -96.92210360129058699 ) ) ;
#8523 = EDGE_CURVE ( 'NONE', #11140, #7745, #958, .T. ) ;
#8524 = EDGE_CURVE ( 'NONE', #694, #2733, #9443, .T. ) ;
#8525 = VERTEX_POINT ( 'NONE', #2839 ) ;
#8526 = CARTESIAN_POINT ( 'NONE',  ( -1018.401127491270358, 110.2021201405460431, -103.3307627799636208 ) ) ;
#8527 = LINE ( 'NONE', #4864, #6057 ) ;
#8528 = CARTESIAN_POINT ( 'NONE',  ( -35.00000000000000000, 163.9999999999999716, 190.3192290001959748 ) ) ;
#8529 = AXIS2_PLACEMENT_3D ( 'NONE', #2568, #528, #10113 ) ;
#8530 = CARTESIAN_POINT ( 'NONE',  ( -1024.691966601154036, 118.8493250655916142, -122.7172756069790580 ) ) ;
#8531 = VERTEX_POINT ( 'NONE', #8528 ) ;
#8532 = DIRECTION ( 'NONE',  ( 0.000000000000000000, 1.000000000000000000, 0.000000000000000000 ) ) ;
#8533 = FACE_OUTER_BOUND ( 'NONE', #1212, .T. ) ;
#8534 = DIRECTION ( 'NONE',  ( -0.000000000000000000, -1.000000000000000000, -1.757987137413040192E-14 ) ) ;
#8535 = CARTESIAN_POINT ( 'NONE',  ( -974.3195816561885749, 116.7169707472886842, -141.4553492942758055 ) ) ;
#8536 =( NAMED_UNIT ( * ) SI_UNIT ( $, .STERADIAN. ) SOLID_ANGLE_UNIT ( ) );
#8537 = CARTESIAN_POINT ( 'NONE',  ( 120.8820948793965186, 12.00000000000000000, -194.1989091883332890 ) ) ;
#8538 = DIRECTION ( 'NONE',  ( 1.000000000000000000, 0.000000000000000000, 0.000000000000000000 ) ) ;
#8539 = CIRCLE ( 'NONE', #3191, 7.500000000000007105 ) ;
#8540 = VERTEX_POINT ( 'NONE', #6421 ) ;
#8541 = CARTESIAN_POINT ( 'NONE',  ( -380.3309181785604665, 99.96675497247912290, -133.5619496204727454 ) ) ;
#8542 = ORIENTED_EDGE ( 'NONE', *, *, #7842, .F. ) ;
#8543 = CYLINDRICAL_SURFACE ( 'NONE', #7349, 7.500000000000007105 ) ;
#8544 = ORIENTED_EDGE ( 'NONE', *, *, #740, .T. ) ;
#8545 = AXIS2_PLACEMENT_3D ( 'NONE', #3120, #331, #10722 ) ;
#8546 = DIRECTION ( 'NONE',  ( 0.000000000000000000, 1.000000000000000000, 0.000000000000000000 ) ) ;
#8547 = CARTESIAN_POINT ( 'NONE',  ( -824.1700714248523809, 73.67466183167414329, -106.4959216872583028 ) ) ;
#8548 = DIRECTION ( 'NONE',  ( -2.040851148208007875E-17, 1.000000000000000000, 0.000000000000000000 ) ) ;
#8549 = CARTESIAN_POINT ( 'NONE',  ( -1038.401083800579045, 57.54275223462362021, -149.7857175106632326 ) ) ;
#8550 = VERTEX_POINT ( 'NONE', #10257 ) ;
#8551 = CARTESIAN_POINT ( 'NONE',  ( -384.8059386751791635, 78.06308572025466219, -144.3338303615605867 ) ) ;
#8552 = CARTESIAN_POINT ( 'NONE',  ( 4.454233577106967753E-15, 166.0000000000000000, -124.6807709998038405 ) ) ;
#8553 = CARTESIAN_POINT ( 'NONE',  ( -384.9624955846592229, 80.33371017125860192, -104.7475307242005869 ) ) ;
#8554 = LINE ( 'NONE', #10281, #2141 ) ;
#8555 = ORIENTED_EDGE ( 'NONE', *, *, #8104, .F. ) ;
#8556 = EDGE_CURVE ( 'NONE', #5849, #7221, #5492, .T. ) ;
#8557 = DIRECTION ( 'NONE',  ( -0.000000000000000000, -1.000000000000000000, -0.000000000000000000 ) ) ;
#8558 = CARTESIAN_POINT ( 'NONE',  ( -975.5821371384171243, 62.83201726680821508, -96.78565065507949328 ) ) ;
#8559 = CARTESIAN_POINT ( 'NONE',  ( 0.000000000000000000, -7.794228634059949812, -4.499999999999995559 ) ) ;
#8560 = DIRECTION ( 'NONE',  ( -1.000000000000000000, 0.000000000000000000, 0.000000000000000000 ) ) ;
#8561 = CARTESIAN_POINT ( 'NONE',  ( -854.0902776497799778, 23.28889115110665742, -122.7172756069793138 ) ) ;
#8562 = ORIENTED_EDGE ( 'NONE', *, *, #1998, .T. ) ;
#8563 = CARTESIAN_POINT ( 'NONE',  ( -383.1733367470700955, 70.62324166987772855, -108.1910793484533997 ) ) ;
#8564 = CARTESIAN_POINT ( 'NONE',  ( 9.371890508914830252E-13, -6.000000000000006217, -28.92135623730948524 ) ) ;
#8565 = ORIENTED_EDGE ( 'NONE', *, *, #6388, .T. ) ;
#8566 = PRODUCT_CONTEXT ( 'NONE', #366, 'mechanical' ) ;
#8567 = ORIENTED_EDGE ( 'NONE', *, *, #8739, .T. ) ;
#8568 = LINE ( 'NONE', #6649, #5856 ) ;
#8569 = CARTESIAN_POINT ( 'NONE',  ( -1057.693846703447207, 44.87596864925360052, -113.1262384684097100 ) ) ;
#8570 = EDGE_CURVE ( 'NONE', #6627, #957, #42, .T. ) ;
#8571 = DIRECTION ( 'NONE',  ( -8.163404592832030268E-17, 1.000000000000000000, -0.000000000000000000 ) ) ;
#8572 = CYLINDRICAL_SURFACE ( 'NONE', #9565, 7.500000000000007105 ) ;
#8573 = ADVANCED_FACE ( 'NONE', ( #1977 ), #5092, .T. ) ;
#8574 = CARTESIAN_POINT ( 'NONE',  ( -852.8684863605125202, 118.0406360202081970, -113.1262384684093405 ) ) ;
#8575 = FACE_BOUND ( 'NONE', #11654, .T. ) ;
#8576 = CARTESIAN_POINT ( 'NONE',  ( -21.02500011264404023, 178.7212721744384396, -125.1324667871970036 ) ) ;
#8577 = AXIS2_PLACEMENT_3D ( 'NONE', #4919, #7524, #216 ) ;
#8578 = CIRCLE ( 'NONE', #6783, 1.000000000000000888 ) ;
#8579 = VERTEX_POINT ( 'NONE', #5977 ) ;
#8580 = CYLINDRICAL_SURFACE ( 'NONE', #661, 7.500000000000012434 ) ;
#8581 = EDGE_LOOP ( 'NONE', ( #5784, #11546 ) ) ;
#8582 = CARTESIAN_POINT ( 'NONE',  ( -3.373308712440251100E-15, -8.014718854569432338, -4.118099735505507120 ) ) ;
#8583 = CARTESIAN_POINT ( 'NONE',  ( -1021.777026427250121, 118.8177985574659346, -130.5712005305405228 ) ) ;
#8584 = CARTESIAN_POINT ( 'NONE',  ( 19.87268743161337170, 178.9255784920988503, -126.9338343023757290 ) ) ;
#8585 = AXIS2_PLACEMENT_3D ( 'NONE', #9674, #9225, #766 ) ;
#8586 = EDGE_CURVE ( 'NONE', #10417, #7974, #10427, .T. ) ;
#8587 = CARTESIAN_POINT ( 'NONE',  ( -1060.773655115450993, 112.4236047030758527, -118.7903414690679682 ) ) ;
#8588 = ORIENTED_EDGE ( 'NONE', *, *, #2496, .F. ) ;
#8589 = CARTESIAN_POINT ( 'NONE',  ( -157.5000000000000000, -9.213203435596451385, -126.4213562373084301 ) ) ;
#8590 = CARTESIAN_POINT ( 'NONE',  ( -82.49999999999997158, 24.00000000000001421, -126.4213562373088564 ) ) ;
#8591 = CARTESIAN_POINT ( 'NONE',  ( -952.1456544189259148, 108.1568929870910836, -149.7857175106632042 ) ) ;
#8592 = EDGE_CURVE ( 'NONE', #6719, #4553, #1290, .T. ) ;
#8593 = AXIS2_PLACEMENT_3D ( 'NONE', #6401, #5054, #10172 ) ;
#8594 = PRESENTATION_STYLE_ASSIGNMENT (( #7605 ) ) ;
#8595 = CIRCLE ( 'NONE', #11754, 7.500000000000013323 ) ;
#8596 = CARTESIAN_POINT ( 'NONE',  ( -90.00000000000000000, 139.9999999999999716, -126.4213562373088564 ) ) ;
#8597 = EDGE_LOOP ( 'NONE', ( #5433, #8200 ) ) ;
#8598 = LINE ( 'NONE', #11436, #1544 ) ;
#8599 = CARTESIAN_POINT ( 'NONE',  ( -372.7918232332913817, 100.6587063813212524, -131.9323245634151647 ) ) ;
#8600 = CARTESIAN_POINT ( 'NONE',  ( -974.4564103291385209, 111.0951925441807759, -146.0307792196441312 ) ) ;
#8601 = FACE_BOUND ( 'NONE', #383, .T. ) ;
#8602 = ORIENTED_EDGE ( 'NONE', *, *, #3078, .T. ) ;
#8603 = ADVANCED_FACE ( 'NONE', ( #4184 ), #400, .F. ) ;
#8604 = AXIS2_PLACEMENT_3D ( 'NONE', #6222, #10106, #3358 ) ;
#8605 = EDGE_LOOP ( 'NONE', ( #4794, #1138, #11320, #9190 ) ) ;
#8606 = B_SPLINE_CURVE_WITH_KNOTS ( 'NONE', 3,
 ( #4568, #11976, #3494, #6345, #10119, #8344, #7408, #3552, #726, #1652, #5412, #11182, #9191, #4504, #7342, #11113, #6478, #10252, #4635, #1786, #5548, #865, #8413, #12176, #3692, #7469, #2774, #6538, #10306, #8760, #7768, #10549, #35, #153, #6659, #5914, #9566, #4921 ),
 .UNSPECIFIED., .F., .F.,
 ( 4, 2, 2, 2, 2, 2, 2, 2, 2, 2, 2, 2, 2, 2, 2, 2, 2, 2, 4 ),
 ( 0.07998895219617635499, 0.08341829896746193185, 0.08513297235310469946, 0.08684764573874746707, 0.09370633928131860690, 0.09713568605260422539, 0.1005650328238898439, 0.1039943795951754624, 0.1057090529808182716, 0.1074237263664610809, 0.1142824199090320403, 0.1177117666803174645, 0.1211411134516029164, 0.1228557868372455869, 0.1245704602228882713, 0.1279998069941736261, 0.1314291537654590225, 0.1331438271511017069, 0.1348585005367443912 ),
 .UNSPECIFIED. ) ;
#8607 = CARTESIAN_POINT ( 'NONE',  ( -126.4213562373094959, 0.000000000000000000, 2.255140518769849223E-14 ) ) ;
#8608 = FACE_BOUND ( 'NONE', #5090, .T. ) ;
#8609 = CARTESIAN_POINT ( 'NONE',  ( -997.0443963278715955, 49.75991663364307271, -146.0307792196450691 ) ) ;
#8610 = ORIENTED_EDGE ( 'NONE', *, *, #9494, .T. ) ;
#8611 = CARTESIAN_POINT ( 'NONE',  ( -374.7039800877403763, 74.36633201333150112, -143.2283958171015854 ) ) ;
#8612 = CARTESIAN_POINT ( 'NONE',  ( -19.03136272649511085, 180.2041921146316668, -134.6807709998038547 ) ) ;
#8613 = CARTESIAN_POINT ( 'NONE',  ( -374.9671836365860713, 79.81299459977714150, -94.78091058644133682 ) ) ;
#8614 = DIRECTION ( 'NONE',  ( 1.000000000000000000, 0.000000000000000000, 0.000000000000000000 ) ) ;
#8615 = AXIS2_PLACEMENT_3D ( 'NONE', #1833, #8267, #850 ) ;
#8616 = ORIENTED_EDGE ( 'NONE', *, *, #2543, .F. ) ;
#8617 = CARTESIAN_POINT ( 'NONE',  ( -976.1667687410277949, 38.51511931708004965, -136.2353035311986957 ) ) ;
#8618 = ORIENTED_EDGE ( 'NONE', *, *, #941, .F. ) ;
#8619 = PRODUCT ( 'Cast Iron Base Mounting Frame', 'Cast Iron Base Mounting Frame', '', ( #1094 ) ) ;
#8620 = CARTESIAN_POINT ( 'NONE',  ( -1032.260242496269029, 61.00429285198274698, -99.57582448894517313 ) ) ;
#8621 = DIRECTION ( 'NONE',  ( -0.000000000000000000, -1.000000000000000000, 0.000000000000000000 ) ) ;
#8622 = DIRECTION ( 'NONE',  ( -1.000000000000000000, -0.000000000000000000, -0.000000000000000000 ) ) ;
#8623 = CARTESIAN_POINT ( 'NONE',  ( -976.2351830774960035, 35.86345807843989775, -130.5712005305402101 ) ) ;
#8624 = EDGE_LOOP ( 'NONE', ( #2148, #7992, #1357, #8062, #8296, #1626 ) ) ;
#8625 = AXIS2_PLACEMENT_3D ( 'NONE', #10040, #11777, #9858 ) ;
#8626 = CARTESIAN_POINT ( 'NONE',  ( -819.3316697785987799, 80.88429704961258437, -144.6519063719970006 ) ) ;
#8627 = CARTESIAN_POINT ( 'NONE',  ( -384.8558507370726147, 78.74686981056612467, -104.9381817955416096 ) ) ;
#8628 = CARTESIAN_POINT ( 'NONE',  ( -828.3150505402204544, 76.46109783575887775, -154.6692737003968148 ) ) ;
#8629 = ORIENTED_EDGE ( 'NONE', *, *, #8039, .F. ) ;
#8630 = VERTEX_POINT ( 'NONE', #5787 ) ;
#8631 = CARTESIAN_POINT ( 'NONE',  ( -997.7839878466058963, 40.27522178589197921, -113.1262384684093547 ) ) ;
#8632 = CARTESIAN_POINT ( 'NONE',  ( -126.4213562373094959, 12.00000000000000000, 2.255140518769849223E-14 ) ) ;
#8633 = CARTESIAN_POINT ( 'NONE',  ( 35.00000000000000000, 11.99999999999998046, 190.3192290001959748 ) ) ;
#8634 = DIRECTION ( 'NONE',  ( 3.061276722312011504E-17, -1.000000000000000000, 0.000000000000000000 ) ) ;
#8635 = AXIS2_PLACEMENT_3D ( 'NONE', #1976, #6371, #688 ) ;
#8636 = PRODUCT_DEFINITION_CONTEXT ( 'detailed design', #4235, 'design' ) ;
#8637 = CARTESIAN_POINT ( 'NONE',  ( -951.7027691703317487, 118.7449601027236241, -107.9061927053324581 ) ) ;
#8638 = FACE_OUTER_BOUND ( 'NONE', #9835, .T. ) ;
#8639 = CARTESIAN_POINT ( 'NONE',  ( -21.06687908627628403, 179.1075766945866121, -125.9428570876586804 ) ) ;
#8640 = EDGE_CURVE ( 'NONE', #11203, #10417, #2529, .T. ) ;
#8641 = ORIENTED_EDGE ( 'NONE', *, *, #9663, .T. ) ;
#8642 = AXIS2_PLACEMENT_3D ( 'NONE', #409, #7916, #10861 ) ;
#8643 = CARTESIAN_POINT ( 'NONE',  ( -374.7080949166565347, 88.40015326679682062, -95.58188032217027796 ) ) ;
#8644 = ADVANCED_FACE ( 'NONE', ( #1113 ), #6907, .F. ) ;
#8645 = AXIS2_PLACEMENT_3D ( 'NONE', #3597, #707, #9040 ) ;
#8646 = ORIENTED_EDGE ( 'NONE', *, *, #544, .T. ) ;
#8647 = CARTESIAN_POINT ( 'NONE',  ( -823.1749794181283733, 110.1592441374100844, -107.9061927053325292 ) ) ;
#8648 = DIRECTION ( 'NONE',  ( -0.000000000000000000, 1.000000000000000000, 7.930164461608263644E-17 ) ) ;
#8649 = DIRECTION ( 'NONE',  ( -8.163404592832030268E-17, 1.000000000000000000, -0.000000000000000000 ) ) ;
#8650 = ADVANCED_FACE ( 'NONE', ( #4073 ), #10734, .F. ) ;
#8651 = PRESENTATION_LAYER_ASSIGNMENT (  '', '', ( #1937 ) ) ;
#8652 = CARTESIAN_POINT ( 'NONE',  ( -1013.875822516560447, 120.2710389253235519, -122.7172756069789017 ) ) ;
#8653 = EDGE_LOOP ( 'NONE', ( #4167, #1991, #9590, #4700 ) ) ;
#8654 = CARTESIAN_POINT ( 'NONE',  ( -823.7697810748812799, 117.7733807739867871, -124.6807709998041531 ) ) ;
#8655 = CARTESIAN_POINT ( 'NONE',  ( -375.0000000000000000, 83.13026420090928070, -94.68077099980384048 ) ) ;
#8656 = CARTESIAN_POINT ( 'NONE',  ( 120.8820948793965186, 12.00000000000000000, -186.6989091883332890 ) ) ;
#8657 = CARTESIAN_POINT ( 'NONE',  ( 0.000000000000000000, 1.502314598737159426E-15, -9.000000000000000000 ) ) ;
#8658 = CARTESIAN_POINT ( 'NONE',  ( -1022.124201078499027, 113.7707856953084189, -141.4553492942762887 ) ) ;
#8659 = DIRECTION ( 'NONE',  ( 0.000000000000000000, 0.000000000000000000, 1.000000000000000000 ) ) ;
#8660 = FACE_OUTER_BOUND ( 'NONE', #1085, .T. ) ;
#8661 = EDGE_LOOP ( 'NONE', ( #4774, #11137 ) ) ;
#8662 = AXIS2_PLACEMENT_3D ( 'NONE', #491, #7307, #8051 ) ;
#8663 = ADVANCED_FACE ( 'NONE', ( #10672 ), #1347, .F. ) ;
#8664 = DIRECTION ( 'NONE',  ( 0.000000000000000000, 0.000000000000000000, -1.000000000000000000 ) ) ;
#8665 = FACE_BOUND ( 'NONE', #9847, .T. ) ;
#8666 = ORIENTED_EDGE ( 'NONE', *, *, #8965, .T. ) ;
#8667 = PRODUCT_RELATED_PRODUCT_CATEGORY ( 'part', '', ( #6637 ) ) ;
#8668 =( REPRESENTATION_RELATIONSHIP ('NONE','NONE', #12149, #1102 ) REPRESENTATION_RELATIONSHIP_WITH_TRANSFORMATION ( #9386 )SHAPE_REPRESENTATION_RELATIONSHIP( ) );
#8669 = VECTOR ( 'NONE', #5620, 1000.000000000000000 ) ;
#8670 = ORIENTED_EDGE ( 'NONE', *, *, #6565, .F. ) ;
#8671 = AXIS2_PLACEMENT_3D ( 'NONE', #10555, #9808, #1228 ) ;
#8672 = DIRECTION ( 'NONE',  ( 0.000000000000000000, 1.000000000000000000, 0.000000000000000000 ) ) ;
#8673 = CARTESIAN_POINT ( 'NONE',  ( -820.0492617104193869, 75.38478674231537013, -105.8049000242702533 ) ) ;
#8674 = CARTESIAN_POINT ( 'NONE',  ( 1.959217102279688941E-15, 139.9999999999999716, -126.4213562373094959 ) ) ;
#8675 = CARTESIAN_POINT ( 'NONE',  ( -853.9759289228051102, 31.63339360934212152, -141.4553492942759192 ) ) ;
#8676 = ORIENTED_EDGE ( 'NONE', *, *, #10025, .T. ) ;
#8677 = CARTESIAN_POINT ( 'NONE',  ( -383.2504773128821398, 70.84834670873947005, -141.3339299216349616 ) ) ;
#8678 = DIRECTION ( 'NONE',  ( 1.000000000000000000, 0.000000000000000000, -0.000000000000000000 ) ) ;
#8679 = CARTESIAN_POINT ( 'NONE',  ( -372.9799184754957082, 65.30137661730785226, -101.5283204515378088 ) ) ;
#8680 = EDGE_CURVE ( 'NONE', #2603, #6447, #3944, .T. ) ;
#8681 = CONICAL_SURFACE ( 'NONE', #4915, 9.000000000000000000, 1.047197551196600296 ) ;
#8682 = ORIENTED_EDGE ( 'NONE', *, *, #9843, .F. ) ;
#8683 = ORIENTED_EDGE ( 'NONE', *, *, #9499, .F. ) ;
#8684 = CARTESIAN_POINT ( 'NONE',  ( -375.0000000000000000, 81.99999999999995737, -89.68077099980384048 ) ) ;
#8685 = CARTESIAN_POINT ( 'NONE',  ( 21.04250863801212290, 178.7733595539146734, -125.3557961042217386 ) ) ;
#8686 = CARTESIAN_POINT ( 'NONE',  ( -1028.259718048105469, 56.21337363619640115, -107.9061927053325434 ) ) ;
#8687 = AXIS2_PLACEMENT_3D ( 'NONE', #8469, #4434, #7275 ) ;
#8688 = CARTESIAN_POINT ( 'NONE',  ( -819.4838385048408327, 81.17047855582200100, -104.6961160549178089 ) ) ;
#8689 = CARTESIAN_POINT ( 'NONE',  ( -1048.334963668468163, 42.40858384259928471, -136.2353035311987242 ) ) ;
#8690 = ORIENTED_EDGE ( 'NONE', *, *, #11312, .F. ) ;
#8691 = CARTESIAN_POINT ( 'NONE',  ( -384.4864278086921558, 75.86462062201600531, -105.6083542711734680 ) ) ;
#8692 = CARTESIAN_POINT ( 'NONE',  ( -824.1535707999410079, 73.67424315034676852, -154.6483812918586125 ) ) ;
#8693 = ORIENTED_EDGE ( 'NONE', *, *, #4070, .T. ) ;
#8694 = APPLICATION_PROTOCOL_DEFINITION ( 'draft international standard', 'automotive_design', 1998, #11822 ) ;
#8695 = VERTEX_POINT ( 'NONE', #348 ) ;
#8696 = CARTESIAN_POINT ( 'NONE',  ( -1062.996098538733122, 47.98024286075321498, -118.7903414690683377 ) ) ;
#8697 = CYLINDRICAL_SURFACE ( 'NONE', #6939, 7.500000000000007105 ) ;
#8698 = CARTESIAN_POINT ( 'NONE',  ( 4.335549520754014653E-15, 167.0000000000000000, -124.6807709998038405 ) ) ;
#8699 = FACE_BOUND ( 'NONE', #8737, .T. ) ;
#8700 = CARTESIAN_POINT ( 'NONE',  ( -19.97345815004482716, 177.8596483071499108, -125.7207219634393311 ) ) ;
#8701 = ORIENTED_EDGE ( 'NONE', *, *, #6780, .T. ) ;
#8702 = CYLINDRICAL_SURFACE ( 'NONE', #1650, 7.500000000000007105 ) ;
#8703 = ORIENTED_EDGE ( 'NONE', *, *, #9458, .T. ) ;
#8704 = CARTESIAN_POINT ( 'NONE',  ( -903.4746773471185861, 104.0883302344921475, -96.78565065507889642 ) ) ;
#8705 = CARTESIAN_POINT ( 'NONE',  ( -795.0000000000038654, 109.8950841424301359, -136.2353035311980136 ) ) ;
#8706 = DIRECTION ( 'NONE',  ( -1.224646799147353207E-16, -1.453460497224676649E-32, 1.000000000000000000 ) ) ;
#8707 = EDGE_CURVE ( 'NONE', #7292, #3585, #11675, .T. ) ;
#8708 = CARTESIAN_POINT ( 'NONE',  ( -951.4198147059589701, 125.0824040815807194, -124.6807709998040252 ) ) ;
#8709 = ORIENTED_EDGE ( 'NONE', *, *, #7667, .F. ) ;
#8710 = CYLINDRICAL_SURFACE ( 'NONE', #7776, 7.500000000000007105 ) ;
#8711 = CARTESIAN_POINT ( 'NONE',  ( -819.8468830326148691, 81.71630402067583532, -104.6809196082601119 ) ) ;
#8712 = CARTESIAN_POINT ( 'NONE',  ( 35.00000000000000000, 2.428612866367529932E-14, -159.6807709998040252 ) ) ;
#8713 = CARTESIAN_POINT ( 'NONE',  ( -1046.261572611719657, 104.4651992465226868, -146.0307792196445575 ) ) ;
#8714 = CIRCLE ( 'NONE', #1591, 8.999999999999998224 ) ;
#8715 = DIRECTION ( 'NONE',  ( 0.000000000000000000, 0.000000000000000000, -1.000000000000000000 ) ) ;
#8716 =( NAMED_UNIT ( * ) SI_UNIT ( $, .STERADIAN. ) SOLID_ANGLE_UNIT ( ) );
#8717 = VERTEX_POINT ( 'NONE', #3189 ) ;
#8718 = DIRECTION ( 'NONE',  ( -1.876626137810916309E-30, -1.000000000000000000, -4.930380657631307143E-31 ) ) ;
#8719 = CARTESIAN_POINT ( 'NONE',  ( -1022.124201078499027, 113.7707856953084189, -141.4553492942762887 ) ) ;
#8720 = AXIS2_PLACEMENT_3D ( 'NONE', #2104, #2963, #6725 ) ;
#8721 = FACE_BOUND ( 'NONE', #601, .T. ) ;
#8722 = EDGE_CURVE ( 'NONE', #3971, #2594, #9046, .T. ) ;
#8723 = EDGE_LOOP ( 'NONE', ( #6572, #3893, #11873, #7875 ) ) ;
#8724 = ORIENTED_EDGE ( 'NONE', *, *, #10993, .T. ) ;
#8725 = AXIS2_PLACEMENT_3D ( 'NONE', #7910, #4870, #9632 ) ;
#8726 = CARTESIAN_POINT ( 'NONE',  ( 2.186774452080127126E-12, -6.000000000000006217, 91.07864376269050410 ) ) ;
#8727 = CARTESIAN_POINT ( 'NONE',  ( -1047.844889418685170, 56.55730854968103927, -149.7857175106634315 ) ) ;
#8728 = CARTESIAN_POINT ( 'NONE',  ( -202.4999999999999716, -9.213203435596478030, -126.4213562373080180 ) ) ;
#8729 = CIRCLE ( 'NONE', #4000, 7.500000000000007105 ) ;
#8730 = CARTESIAN_POINT ( 'NONE',  ( -374.9896482698936779, 80.71982717203331958, -154.6492122816839299 ) ) ;
#8731 = DIRECTION ( 'NONE',  ( 1.000000000000000000, 0.000000000000000000, 0.000000000000000000 ) ) ;
#8732 = CARTESIAN_POINT ( 'NONE',  ( -374.9143915958317166, 78.51216652322804634, -94.94260781757940038 ) ) ;
#8733 =( LENGTH_UNIT ( ) NAMED_UNIT ( * ) SI_UNIT ( .MILLI., .METRE. ) );
#8734 = DIRECTION ( 'NONE',  ( 0.000000000000000000, 1.000000000000000000, 0.000000000000000000 ) ) ;
#8735 = VERTEX_POINT ( 'NONE', #3076 ) ;
#8736 = AXIS2_PLACEMENT_3D ( 'NONE', #3377, #479, #6241 ) ;
#8737 = EDGE_LOOP ( 'NONE', ( #8347, #4742 ) ) ;
#8738 = CARTESIAN_POINT ( 'NONE',  ( 19.99986396686996670, 178.6891417861111790, -124.8519595561770359 ) ) ;
#8739 = EDGE_CURVE ( 'NONE', #569, #8373, #3509, .T. ) ;
#8740 = CARTESIAN_POINT ( 'NONE',  ( -1014.107508992752514, 52.59077491224128664, -118.7903414690682951 ) ) ;
#8741 = CARTESIAN_POINT ( 'NONE',  ( -19.99905741042869423, 182.7066083885001149, -124.9054265645020365 ) ) ;
#8742 = CARTESIAN_POINT ( 'NONE',  ( -19.96332333990081764, 180.6948238841417265, -123.2561630805032848 ) ) ;
#8743 = ORIENTED_EDGE ( 'NONE', *, *, #7308, .T. ) ;
#8744 = CARTESIAN_POINT ( 'NONE',  ( -379.8999661783463466, 63.26100480178833863, -117.6669381337575544 ) ) ;
#8745 = ORIENTED_EDGE ( 'NONE', *, *, #4565, .T. ) ;
#8746 = DIRECTION ( 'NONE',  ( 0.000000000000000000, 0.000000000000000000, 1.000000000000000000 ) ) ;
#8747 = CIRCLE ( 'NONE', #11894, 7.500000000000007105 ) ;
#8748 = EDGE_LOOP ( 'NONE', ( #4503, #10534, #9765, #5974 ) ) ;
#8749 = EDGE_CURVE ( 'NONE', #1654, #8525, #2943, .T. ) ;
#8750 = PRODUCT_CONTEXT ( 'NONE', #10713, 'mechanical' ) ;
#8751 = ORIENTED_EDGE ( 'NONE', *, *, #2319, .F. ) ;
#8752 = CARTESIAN_POINT ( 'NONE',  ( -854.0803342822198374, 23.97549884981706825, -118.7903414690682808 ) ) ;
#8753 = CARTESIAN_POINT ( 'NONE',  ( -35.00000000000000000, 152.0000000000000000, -124.6807709998038689 ) ) ;
#8754 = AXIS2_PLACEMENT_3D ( 'NONE', #11745, #3259, #7037 ) ;
#8755 = EDGE_CURVE ( 'NONE', #8579, #915, #7774, .T. ) ;
#8756 = CARTESIAN_POINT ( 'NONE',  ( -853.1108559448483675, 99.60875591605646662, -99.57582448894477523 ) ) ;
#8757 = DIRECTION ( 'NONE',  ( 3.061276722312011504E-17, -1.000000000000000000, -0.000000000000000000 ) ) ;
#8758 = CARTESIAN_POINT ( 'NONE',  ( -19.88457985033570097, 178.7457540148283499, -126.8279919963933509 ) ) ;
#8759 = EDGE_LOOP ( 'NONE', ( #1744, #1607, #2434, #11665, #2265, #2961, #4595, #8542, #2114, #758 ) ) ;
#8760 = CARTESIAN_POINT ( 'NONE',  ( -374.4501075384643514, 73.18187568907286789, -152.9657676401715491 ) ) ;
#8761 = AXIS2_PLACEMENT_3D ( 'NONE', #9983, #3299, #8072 ) ;
#8762 = ORIENTED_EDGE ( 'NONE', *, *, #8441, .T. ) ;
#8763 = CARTESIAN_POINT ( 'NONE',  ( -952.6992609796628813, 94.45070821374962122, -95.06748246947989855 ) ) ;
#8764 = ORIENTED_EDGE ( 'NONE', *, *, #2772, .T. ) ;
#8765 = CARTESIAN_POINT ( 'NONE',  ( -991.8293279264742068, 119.7328159579556086, -136.2353035311976726 ) ) ;
#8766 = AXIS2_PLACEMENT_3D ( 'NONE', #1010, #6569, #8498 ) ;
#8767 = TOROIDAL_SURFACE ( 'NONE', #76, 6.599999999999998757, 0.5999999999999999778 ) ;
#8768 = ORIENTED_EDGE ( 'NONE', *, *, #105, .T. ) ;
#8769 = CARTESIAN_POINT ( 'NONE',  ( -795.0000000000047748, 112.0000000000007532, -124.6807709998042384 ) ) ;
#8770 = CARTESIAN_POINT ( 'NONE',  ( -821.6103028745218353, 83.16718542005921222, -104.7144644823254822 ) ) ;
#8771 = FACE_BOUND ( 'NONE', #1831, .T. ) ;
#8772 = CARTESIAN_POINT ( 'NONE',  ( -1011.418100375194967, 110.6663390795549162, -146.0307792196444723 ) ) ;
#8773 = DIRECTION ( 'NONE',  ( -1.186840563529527301E-16, 1.000000000000000000, -0.000000000000000000 ) ) ;
#8774 = ORIENTED_EDGE ( 'NONE', *, *, #6014, .T. ) ;
#8775 = CARTESIAN_POINT ( 'NONE',  ( 6.500000000000030198, -7.999999999999979572, -124.6807709998038405 ) ) ;
#8776 = AXIS2_PLACEMENT_3D ( 'NONE', #1600, #4584, #7481 ) ;
#8777 = CIRCLE ( 'NONE', #1668, 5.999999999999999112 ) ;
#8778 = AXIS2_PLACEMENT_3D ( 'NONE', #3737, #10475, #11464 ) ;
#8779 = CARTESIAN_POINT ( 'NONE',  ( 19.03136272649511085, 180.2041921146316668, -134.6807709998038547 ) ) ;
#8780 = LINE ( 'NONE', #6736, #9520 ) ;
#8781 = VERTEX_POINT ( 'NONE', #9745 ) ;
#8782 = VERTEX_POINT ( 'NONE', #10467 ) ;
#8783 = CIRCLE ( 'NONE', #2275, 7.500000000000013323 ) ;
#8784 = CARTESIAN_POINT ( 'NONE',  ( -822.1919554870401043, 73.93830887977168231, -106.3769876045757599 ) ) ;
#8785 = CARTESIAN_POINT ( 'NONE',  ( -953.5758047008371250, 72.53746257253824581, -152.5758913445294525 ) ) ;
#8786 = CARTESIAN_POINT ( 'NONE',  ( -818.8285638327238303, 78.34153296655600229, -144.3462106687113646 ) ) ;
#8787 = EDGE_LOOP ( 'NONE', ( #8514, #277, #3621, #5369 ) ) ;
#8788 = ADVANCED_FACE ( 'NONE', ( #6253 ), #3275, .F. ) ;
#8789 = CARTESIAN_POINT ( 'NONE',  ( -45.00000000000000000, 25.00000000000002132, -126.4213562373094959 ) ) ;
#8790 = DIRECTION ( 'NONE',  ( 3.061276722312011504E-17, -1.000000000000000000, 0.000000000000000000 ) ) ;
#8791 = CARTESIAN_POINT ( 'NONE',  ( -381.0053422273798560, 65.34300945855264331, -113.5331703338095082 ) ) ;
#8792 = EDGE_CURVE ( 'NONE', #9472, #10481, #3731, .T. ) ;
#8793 = CARTESIAN_POINT ( 'NONE',  ( 0.000000000000000000, 12.00000000000000000, -264.6807709998040536 ) ) ;
#8794 = CARTESIAN_POINT ( 'NONE',  ( -928.4218612484578443, 59.99049470396625594, -130.5712005305400965 ) ) ;
#8795 = VECTOR ( 'NONE', #589, 1000.000000000000000 ) ;
#8796 = ORIENTED_EDGE ( 'NONE', *, *, #6083, .F. ) ;
#8797 = EDGE_CURVE ( 'NONE', #10145, #4052, #3000, .T. ) ;
#8798 = CARTESIAN_POINT ( 'NONE',  ( -1063.013736978595944, 47.55218547899807646, -122.7172756069792570 ) ) ;
#8799 = FACE_OUTER_BOUND ( 'NONE', #6891, .T. ) ;
#8800 = EDGE_LOOP ( 'NONE', ( #9907, #7779 ) ) ;
#8801 = CARTESIAN_POINT ( 'NONE',  ( -372.7937968025734108, 63.34872752676778873, -117.4098597798181629 ) ) ;
#8802 = CYLINDRICAL_SURFACE ( 'NONE', #5584, 7.500000000000007105 ) ;
#8803 = VERTEX_POINT ( 'NONE', #5770 ) ;
#8804 = CARTESIAN_POINT ( 'NONE',  ( -827.8047116257844209, 75.62532219084948792, -154.6806748490619725 ) ) ;
#8805 = ORIENTED_EDGE ( 'NONE', *, *, #3976, .T. ) ;
#8806 = DIRECTION ( 'NONE',  ( 0.9501779778103254248, 0.000000000000000000, 0.3117078928809486338 ) ) ;
#8807 = ORIENTED_EDGE ( 'NONE', *, *, #2581, .T. ) ;
#8808 = CARTESIAN_POINT ( 'NONE',  ( -976.1667687410197232, 38.51511931707989334, -113.1262384684093263 ) ) ;
#8809 = EDGE_CURVE ( 'NONE', #10118, #7042, #6704, .T. ) ;
#8810 = FACE_OUTER_BOUND ( 'NONE', #1497, .T. ) ;
#8811 =( GEOMETRIC_REPRESENTATION_CONTEXT ( 3 ) GLOBAL_UNCERTAINTY_ASSIGNED_CONTEXT ( ( #2951 ) ) GLOBAL_UNIT_ASSIGNED_CONTEXT ( ( #969, #2014, #2944 ) ) REPRESENTATION_CONTEXT ( 'NONE', 'WORKASPACE' ) );
#8812 = UNCERTAINTY_MEASURE_WITH_UNIT (LENGTH_MEASURE( 1.000000000000000082E-05 ), #2722, 'distance_accuracy_value', 'NONE');
#8813 = CARTESIAN_POINT ( 'NONE',  ( -903.8503739047830550, 115.2915043052427535, -103.3307627799633082 ) ) ;
#8814 = DIRECTION ( 'NONE',  ( -1.000000000000000000, 0.000000000000000000, 0.000000000000000000 ) ) ;
#8815 = ORIENTED_EDGE ( 'NONE', *, *, #6928, .T. ) ;
#8816 = DIRECTION ( 'NONE',  ( -1.000000000000000000, 0.000000000000000000, 0.000000000000000000 ) ) ;
#8817 = FACE_OUTER_BOUND ( 'NONE', #10835, .T. ) ;
#8818 = ORIENTED_EDGE ( 'NONE', *, *, #635, .T. ) ;
#8819 = CARTESIAN_POINT ( 'NONE',  ( -1061.468168685228193, 92.73456844357777129, -96.78565065507918064 ) ) ;
#8820 = CIRCLE ( 'NONE', #4289, 35.00000000000002842 ) ;
#8821 = ADVANCED_FACE ( 'NONE', ( #10762 ), #1492, .T. ) ;
#8822 = ORIENTED_EDGE ( 'NONE', *, *, #10394, .F. ) ;
#8823 = CARTESIAN_POINT ( 'NONE',  ( 4.808665244885994618E-14, -6.000000000000000000, 141.4213562373094817 ) ) ;
#8824 = DIRECTION ( 'NONE',  ( 1.000000000000000000, 0.000000000000000000, 0.000000000000000000 ) ) ;
#8825 = CARTESIAN_POINT ( 'NONE',  ( 1.561981751485805177E-12, -6.000000000000005329, 23.57864376269050410 ) ) ;
#8826 = LINE ( 'NONE', #9749, #9604 ) ;
#8827 = CARTESIAN_POINT ( 'NONE',  ( -818.8614429351425770, 78.01598473359217678, -144.2826642275888105 ) ) ;
#8828 = CIRCLE ( 'NONE', #1335, 7.500000000000007105 ) ;
#8829 = DIRECTION ( 'NONE',  ( -8.163404592832031500E-17, 1.000000000000000000, 0.000000000000000000 ) ) ;
#8830 = DIRECTION ( 'NONE',  ( 0.000000000000000000, 1.000000000000000000, 0.000000000000000000 ) ) ;
#8831 = FACE_BOUND ( 'NONE', #2789, .T. ) ;
#8832 = ORIENTED_EDGE ( 'NONE', *, *, #11394, .T. ) ;
#8833 = CARTESIAN_POINT ( 'NONE',  ( -126.4213562373094959, -6.000000000000000000, 2.255140518769849223E-14 ) ) ;
#8834 = DIRECTION ( 'NONE',  ( 0.000000000000000000, 0.000000000000000000, 1.000000000000000000 ) ) ;
#8835 = CARTESIAN_POINT ( 'NONE',  ( 126.4213562373094959, 0.000000000000000000, -6.938893903907228378E-15 ) ) ;
#8836 = AXIS2_PLACEMENT_3D ( 'NONE', #7624, #7560, #4783 ) ;
#8837 = CARTESIAN_POINT ( 'NONE',  ( -87.04832655144203102, 12.00000000000000000, -217.9289243767376831 ) ) ;
#8838 = VERTEX_POINT ( 'NONE', #5070 ) ;
#8839 = DIRECTION ( 'NONE',  ( -8.163404592832030268E-17, 1.000000000000000000, -0.000000000000000000 ) ) ;
#8840 = EDGE_LOOP ( 'NONE', ( #9331, #8567 ) ) ;
#8841 = ADVANCED_BREP_SHAPE_REPRESENTATION ( '', ( #3860, #11957 ), #5231 ) ;
#8842 = CARTESIAN_POINT ( 'NONE',  ( -821.2975544693643997, 74.34970510072432148, -106.2007125858228704 ) ) ;
#8843 = CARTESIAN_POINT ( 'NONE',  ( -1065.000000000002956, 76.10956187831469322, -154.2940595301282087 ) ) ;
#8844 = VECTOR ( 'NONE', #2902, 1000.000000000000000 ) ;
#8845 = CARTESIAN_POINT ( 'NONE',  ( 1.414009460465297036E-14, -9.213203435596451385, -126.4213562373094959 ) ) ;
#8846 = CARTESIAN_POINT ( 'NONE',  ( -210.0000000000000000, 24.00000000000000711, -126.4213562373080180 ) ) ;
#8847 = CARTESIAN_POINT ( 'NONE',  ( -828.8285638327251945, 78.34868723465601192, -94.76039716391075274 ) ) ;
#8848 = DIRECTION ( 'NONE',  ( -0.000000000000000000, 1.000000000000000000, -0.000000000000000000 ) ) ;
#8849 = CARTESIAN_POINT ( 'NONE',  ( 0.000000000000000000, 12.00000000000000000, -89.68077099980401101 ) ) ;
#8850 = CIRCLE ( 'NONE', #3122, 1.000000000000005773 ) ;
#8851 = VECTOR ( 'NONE', #421, 1000.000000000000000 ) ;
#8852 = VERTEX_POINT ( 'NONE', #8107 ) ;
#8853 = ADVANCED_FACE ( 'NONE', ( #2475 ), #7176, .F. ) ;
#8854 = EDGE_CURVE ( 'NONE', #5617, #8131, #8070, .T. ) ;
#8855 = CARTESIAN_POINT ( 'NONE',  ( -854.0803342822198374, 23.97549884981706825, -118.7903414690682808 ) ) ;
#8856 = DIRECTION ( 'NONE',  ( -0.000000000000000000, -1.000000000000000000, -0.000000000000000000 ) ) ;
#8857 = CARTESIAN_POINT ( 'NONE',  ( -370.0761506609951539, 56.20937627747883880, -118.7459503409855301 ) ) ;
#8858 = AXIS2_PLACEMENT_3D ( 'NONE', #11198, #6640, #7540 ) ;
#8859 = CARTESIAN_POINT ( 'NONE',  ( -382.0049300299783681, 96.47769172040968044, -110.8343367138896838 ) ) ;
#8860 = CARTESIAN_POINT ( 'NONE',  ( -22.49999999999997868, 12.00000000000001776, -126.4213562373092685 ) ) ;
#8861 = VERTEX_POINT ( 'NONE', #10820 ) ;
#8862 = ORIENTED_EDGE ( 'NONE', *, *, #11586, .F. ) ;
#8863 = CARTESIAN_POINT ( 'NONE',  ( -795.0000000000020464, 54.10491585757070965, -113.1262384684093121 ) ) ;
#8864 = CARTESIAN_POINT ( 'NONE',  ( 0.3593302862866777914, 3.504574740661188237, -9.000000000000001776 ) ) ;
#8865 = DIRECTION ( 'NONE',  ( -1.000000000000000000, 0.000000000000000000, 0.000000000000000000 ) ) ;
#8866 = COLOUR_RGB ( '', 0.31764706, 0.68627451, 0.89019608) ;
#8867 = EDGE_CURVE ( 'NONE', #10381, #2733, #11818, .T. ) ;
#8868 = CARTESIAN_POINT ( 'NONE',  ( -1031.476138302181198, 95.34216976508436403, -96.78565065507929432 ) ) ;
#8869 = DIRECTION ( 'NONE',  ( -8.163404592832030268E-17, 1.000000000000000000, -0.000000000000000000 ) ) ;
#8870 = EDGE_CURVE ( 'NONE', #5951, #2669, #2296, .T. ) ;
#8871 = ORIENTED_EDGE ( 'NONE', *, *, #4356, .T. ) ;
#8872 = ORIENTED_EDGE ( 'NONE', *, *, #6747, .F. ) ;
#8873 = CARTESIAN_POINT ( 'NONE',  ( -1037.656130532294128, 99.96792753513312846, -99.57582448894522997 ) ) ;
#8874 = CARTESIAN_POINT ( 'NONE',  ( -35.00000000000000000, 163.9999999999999716, 190.3192290001959748 ) ) ;
#8875 = CARTESIAN_POINT ( 'NONE',  ( -991.6207251904210125, 122.2801902404846714, -130.5712005305406080 ) ) ;
#8876 = CARTESIAN_POINT ( 'NONE',  ( -974.1288507787422759, 124.2142274477005657, -124.6807709998040110 ) ) ;
#8877 = CARTESIAN_POINT ( 'NONE',  ( 7.500000000000000000, 10.39230484541326938, 0.000000000000000000 ) ) ;
#8878 = CARTESIAN_POINT ( 'NONE',  ( -120.0000000000000000, 152.0000000000000000, -126.4213562373086575 ) ) ;
#8879 = DIRECTION ( 'NONE',  ( -1.000000000000000000, -0.000000000000000000, 0.000000000000000000 ) ) ;
#8880 = EDGE_CURVE ( 'NONE', #7697, #11231, #5189, .T. ) ;
#8881 = EDGE_CURVE ( 'NONE', #140, #5809, #5117, .T. ) ;
#8882 = CARTESIAN_POINT ( 'NONE',  ( -828.3277261219641332, 80.87986238895008739, -104.7098637035477964 ) ) ;
#8883 = DIRECTION ( 'NONE',  ( 0.000000000000000000, 0.000000000000000000, 1.000000000000000000 ) ) ;
#8884 = DIRECTION ( 'NONE',  ( 1.000000000000000000, -0.000000000000000000, -0.000000000000000000 ) ) ;
#8885 = VERTEX_POINT ( 'NONE', #8306 ) ;
#8886 = DIRECTION ( 'NONE',  ( -0.000000000000000000, -1.000000000000000000, -0.000000000000000000 ) ) ;
#8887 = PLANE ( 'NONE',  #8754 ) ;
#8888 = CARTESIAN_POINT ( 'NONE',  ( -120.8820948793972434, 12.00000000000000000, -194.1989091883324363 ) ) ;
#8889 = PLANE ( 'NONE',  #9908 ) ;
#8890 = EDGE_LOOP ( 'NONE', ( #252, #624 ) ) ;
#8891 = ORIENTED_EDGE ( 'NONE', *, *, #9101, .T. ) ;
#8892 = CIRCLE ( 'NONE', #3972, 7.500000000000007105 ) ;
#8893 = CARTESIAN_POINT ( 'NONE',  ( -384.7383783008219211, 77.53302683473108914, -144.2117537804176095 ) ) ;
#8894 = CARTESIAN_POINT ( 'NONE',  ( -373.4439786919718927, 96.68931900664449586, -149.5563464679744072 ) ) ;
#8895 = DIRECTION ( 'NONE',  ( -1.000000000000000000, 0.000000000000000000, 0.000000000000000000 ) ) ;
#8896 = CARTESIAN_POINT ( 'NONE',  ( -825.4444756108113097, 73.93131618268111538, -94.70140411087349719 ) ) ;
#8897 = EDGE_LOOP ( 'NONE', ( #5855, #11069 ) ) ;
#8898 = CARTESIAN_POINT ( 'NONE',  ( -997.0443963278715955, 49.75991663364307271, -146.0307792196450691 ) ) ;
#8899 = AXIS2_PLACEMENT_3D ( 'NONE', #777, #11960, #11228 ) ;
#8900 = ORIENTED_EDGE ( 'NONE', *, *, #8524, .T. ) ;
#8901 = EDGE_LOOP ( 'NONE', ( #4160, #8214, #10596, #3616, #6598, #10525 ) ) ;
#8902 = CIRCLE ( 'NONE', #3573, 9.000000000000000000 ) ;
#8903 = CARTESIAN_POINT ( 'NONE',  ( -928.3598895237944362, 61.90886769853011629, -113.1262384684093831 ) ) ;
#8904 = DIRECTION ( 'NONE',  ( 1.000000000000000000, 0.000000000000000000, 0.000000000000000000 ) ) ;
#8905 = CARTESIAN_POINT ( 'NONE',  ( -826.3335398377358842, 83.00469051230240325, -95.17874826138289279 ) ) ;
#8906 = DIRECTION ( 'NONE',  ( 0.000000000000000000, 0.000000000000000000, 1.000000000000000000 ) ) ;
#8907 = ORIENTED_EDGE ( 'NONE', *, *, #2654, .T. ) ;
#8908 = EDGE_CURVE ( 'NONE', #4868, #6384, #9282, .T. ) ;
#8909 = CIRCLE ( 'NONE', #12090, 7.500000000000007105 ) ;
#8910 = ORIENTED_EDGE ( 'NONE', *, *, #9478, .F. ) ;
#8911 = CIRCLE ( 'NONE', #848, 7.500000000000007105 ) ;
#8912 = DIRECTION ( 'NONE',  ( 0.000000000000000000, 0.000000000000000000, -1.000000000000000000 ) ) ;
#8913 = CARTESIAN_POINT ( 'NONE',  ( 20.81144718909768798, 181.2532700293135974, -123.7022494633698102 ) ) ;
#8914 = DIRECTION ( 'NONE',  ( -0.000000000000000000, 1.189524669241239115E-16, -1.000000000000000000 ) ) ;
#8915 = CARTESIAN_POINT ( 'NONE',  ( -952.4132309232843454, 101.5728619241205450, -96.78565065507918064 ) ) ;
#8916 = DIRECTION ( 'NONE',  ( 0.000000000000000000, 1.000000000000000000, 0.000000000000000000 ) ) ;
#8917 = CIRCLE ( 'NONE', #3020, 45.00000000000001421 ) ;
#8918 = VERTEX_POINT ( 'NONE', #2534 ) ;
#8919 = CARTESIAN_POINT ( 'NONE',  ( 126.4213562373094959, 0.000000000000000000, -6.938893903907228378E-15 ) ) ;
#8920 = ADVANCED_FACE ( 'NONE', ( #3515 ), #4592, .F. ) ;
#8921 = SHAPE_REPRESENTATION_RELATIONSHIP ( 'NONE' , 'NONE' ,  #6140, #2640 ) ;
#8922 = EDGE_LOOP ( 'NONE', ( #3091, #1684 ) ) ;
#8923 = CARTESIAN_POINT ( 'NONE',  ( 0.000000000000000000, 24.00000000000001776, -89.68077099980384048 ) ) ;
#8925 = EDGE_CURVE ( 'NONE', #7221, #11989, #7489, .T. ) ;
#8924 = CARTESIAN_POINT ( 'NONE',  ( -1023.463303304735291, 92.47874188371200432, -95.06748246948023962 ) ) ;
#8926 = CARTESIAN_POINT ( 'NONE',  ( 6.247927005943220505E-13, 164.0000000000000000, -66.42135623730948168 ) ) ;
#8927 = CARTESIAN_POINT ( 'NONE',  ( -795.0000000000047748, 112.0000000000007532, -124.6807709998042384 ) ) ;
#8928 = FACE_OUTER_BOUND ( 'NONE', #11751, .T. ) ;
#8929 = CARTESIAN_POINT ( 'NONE',  ( 19.97592758413811254, 178.0092090781685670, -123.6846453938936747 ) ) ;
#8930 = EDGE_CURVE ( 'NONE', #2603, #8317, #9838, .T. ) ;
#8931 = CARTESIAN_POINT ( 'NONE',  ( -954.0688428831313104, 124.4732772249355577, -118.7903414690677693 ) ) ;
#8932 = LINE ( 'NONE', #11676, #7294 ) ;
#8933 = VECTOR ( 'NONE', #9682, 1000.000000000000000 ) ;
#8934 = CARTESIAN_POINT ( 'NONE',  ( -126.4213562373094959, 12.00000000000000000, -7.499999999999991118 ) ) ;
#8935 = CARTESIAN_POINT ( 'NONE',  ( 28.00000000000000000, -492.9999999999998863, -27.99999999999999645 ) ) ;
#8936 = CARTESIAN_POINT ( 'NONE',  ( 21.05748054007814218, 178.8679675183088875, -125.6049322330816409 ) ) ;
#8937 = DIRECTION ( 'NONE',  ( 3.061276722312011504E-17, -1.000000000000000000, 0.000000000000000000 ) ) ;
#8938 = ORIENTED_EDGE ( 'NONE', *, *, #2907, .T. ) ;
#8939 = DIRECTION ( 'NONE',  ( 1.000000000000000000, 0.000000000000000000, 0.000000000000000000 ) ) ;
#8940 = CARTESIAN_POINT ( 'NONE',  ( -991.5701548301636876, 122.8678427087060214, -124.6807709998040536 ) ) ;
#8941 = DIRECTION ( 'NONE',  ( -0.000000000000000000, -1.000000000000000000, -1.757987137413040192E-14 ) ) ;
#8942 = CARTESIAN_POINT ( 'NONE',  ( -87.04832655144203102, 12.00000000000000000, -225.4289243767377116 ) ) ;
#8943 = AXIS2_PLACEMENT_3D ( 'NONE', #7954, #10790, #10668 ) ;
#8944 = EDGE_CURVE ( 'NONE', #11420, #7745, #820, .T. ) ;
#8945 = VECTOR ( 'NONE', #5133, 1000.000000000000000 ) ;
#8946 = DIRECTION ( 'NONE',  ( -1.000000000000000000, -0.000000000000000000, -0.000000000000000000 ) ) ;
#8947 = B_SPLINE_CURVE_WITH_KNOTS ( 'NONE', 3,
 ( #11925, #10695, #9891, #2523, #12122, #3633, #9333, #7418, #7296, #11059, #2718, #873, #12186, #9396, #5793, #11306, #6611, #10618, #8654, #8769 ),
 .UNSPECIFIED., .F., .F.,
 ( 4, 1, 1, 1, 2, 1, 1, 1, 2, 2, 2, 2, 4 ),
 ( 0.000000000000000000, 0.04762575996673557022, 0.07143863995010346635, 0.09525151993347125146, 0.1428772799002068217, 0.1647615404280894369, 0.1757036706920307445, 0.1866458009559719411, 0.2085300614838545563, 0.4016963878702066726, 0.4307237013227157574, 0.6771470142487683308, 1.000000000000000000 ),
 .UNSPECIFIED. ) ;
#8948 = VERTEX_POINT ( 'NONE', #2790 ) ;
#8949 = CIRCLE ( 'NONE', #3620, 44.00000000000001421 ) ;
#8950 = EDGE_LOOP ( 'NONE', ( #12220, #4739, #5143, #5139 ) ) ;
#8951 = CARTESIAN_POINT ( 'NONE',  ( 20.74704732419727193, 179.6356684247163571, -123.4191576945881224 ) ) ;
#8952 = EDGE_CURVE ( 'NONE', #6215, #338, #4529, .T. ) ;
#8953 = CARTESIAN_POINT ( 'NONE',  ( 0.000000000000000000, 12.00000000000001776, -159.6807709998038547 ) ) ;
#8954 = CARTESIAN_POINT ( 'NONE',  ( -818.8614429351464423, 78.01598473359253205, -144.2826642275891800 ) ) ;
#8955 = CIRCLE ( 'NONE', #3627, 7.500000000000007105 ) ;
#8956 = ORIENTED_EDGE ( 'NONE', *, *, #401, .T. ) ;
#8957 = CIRCLE ( 'NONE', #1874, 44.00000000000000711 ) ;
#8958 = CARTESIAN_POINT ( 'NONE',  ( -375.0000000000000568, 81.99999999999994316, -154.6807709998039115 ) ) ;
#8959 = CARTESIAN_POINT ( 'NONE',  ( 0.8038475772933552088, -5.196152422706605378, 8.999999999999998224 ) ) ;
#8960 = CIRCLE ( 'NONE', #6608, 7.500000000000007105 ) ;
#8961 = DIRECTION ( 'NONE',  ( 0.000000000000000000, 0.000000000000000000, 1.000000000000000000 ) ) ;
#8962 = DIRECTION ( 'NONE',  ( 0.000000000000000000, 0.5118973767283547804, 0.8590466085717518574 ) ) ;
#8963 = ORIENTED_EDGE ( 'NONE', *, *, #10141, .T. ) ;
#8964 = CARTESIAN_POINT ( 'NONE',  ( -1057.036663358150690, 58.23757105449725913, -149.7857175106634884 ) ) ;
#8965 = EDGE_CURVE ( 'NONE', #125, #5383, #11630, .T. ) ;
#8966 = ORIENTED_EDGE ( 'NONE', *, *, #5400, .F. ) ;
#8967 = AXIS2_PLACEMENT_3D ( 'NONE', #5629, #939, #749 ) ;
#8968 = CIRCLE ( 'NONE', #4055, 8.500000000000035527 ) ;
#8969 = CARTESIAN_POINT ( 'NONE',  ( -19.98030737385957423, 179.4757119253121402, -125.9751133749524712 ) ) ;
#8970 = DIRECTION ( 'NONE',  ( -1.186840563529527301E-16, 1.000000000000000000, -0.000000000000000000 ) ) ;
#8971 = FACE_OUTER_BOUND ( 'NONE', #9009, .T. ) ;
#8972 = DIRECTION ( 'NONE',  ( -0.000000000000000000, 0.000000000000000000, 1.000000000000000000 ) ) ;
#8973 = ORIENTED_EDGE ( 'NONE', *, *, #7693, .T. ) ;
#8974 = CARTESIAN_POINT ( 'NONE',  ( -826.8798817544267195, 82.64869829037840532, -95.13516794514535491 ) ) ;
#8975 = CARTESIAN_POINT ( 'NONE',  ( -380.4056020936891969, 99.82458448124143047, -115.5361751508218759 ) ) ;
#8976 = ORIENTED_EDGE ( 'NONE', *, *, #3203, .T. ) ;
#8977 = CIRCLE ( 'NONE', #9972, 69.99999999999998579 ) ;
#8978 = ORIENTED_EDGE ( 'NONE', *, *, #2903, .T. ) ;
#8979 = CARTESIAN_POINT ( 'NONE',  ( -305.0000000000000568, 139.9999999999999716, -159.6807709998038547 ) ) ;
#8980 = CARTESIAN_POINT ( 'NONE',  ( -217.5000000000000000, 151.9999999999999716, -126.4213562373080180 ) ) ;
#8981 = CARTESIAN_POINT ( 'NONE',  ( -1018.692594135739682, 105.1726068785156656, -99.57582448894508786 ) ) ;
#8982 = DIRECTION ( 'NONE',  ( -1.000000000000000000, -3.061276722312011504E-17, -0.000000000000000000 ) ) ;
#8983 = VERTEX_POINT ( 'NONE', #2728 ) ;
#8984 = FACE_OUTER_BOUND ( 'NONE', #10275, .T. ) ;
#8985 = SHAPE_REPRESENTATION_RELATIONSHIP ( 'NONE' , 'NONE' ,  #3601, #3830 ) ;
#8986 = ORIENTED_EDGE ( 'NONE', *, *, #10817, .F. ) ;
#8987 = DIRECTION ( 'NONE',  ( -1.000000000000000000, 0.000000000000000000, 0.000000000000000000 ) ) ;
#8988 = SHAPE_REPRESENTATION_RELATIONSHIP ( 'NONE' , 'NONE' ,  #6213, #7064 ) ;
#8989 = CARTESIAN_POINT ( 'NONE',  ( 87.04832655144112152, 12.00000000000000000, -217.9289243767383368 ) ) ;
#8990 = ORIENTED_EDGE ( 'NONE', *, *, #11746, .F. ) ;
#8991 = DIRECTION ( 'NONE',  ( -0.000000000000000000, 0.000000000000000000, -1.000000000000000000 ) ) ;
#8992 = CARTESIAN_POINT ( 'NONE',  ( -1062.301584968951602, 67.66927912025059300, -96.78565065507969223 ) ) ;
#8993 = CARTESIAN_POINT ( 'NONE',  ( 4.255174644013695128E-15, 25.00000000000002132, -126.4213562373094959 ) ) ;
#8994 = CARTESIAN_POINT ( 'NONE',  ( -21.06729583384051097, 179.4139655881280078, -126.1965993184190040 ) ) ;
#8995 = CARTESIAN_POINT ( 'NONE',  ( -1021.743962174751232, 119.2557508373790824, -126.6442663926290209 ) ) ;
#8996 = ADVANCED_FACE ( 'NONE', ( #10324, #2662 ), #7306, .T. ) ;
#8997 = DIRECTION ( 'NONE',  ( 0.000000000000000000, 1.000000000000000000, 0.000000000000000000 ) ) ;
#8998 = EDGE_CURVE ( 'NONE', #2717, #20, #6497, .T. ) ;
#8999 = FACE_BOUND ( 'NONE', #8156, .T. ) ;
#9000 = CARTESIAN_POINT ( 'NONE',  ( -270.0000000000000000, 139.9999999999999716, -126.4213562373076059 ) ) ;
#9001 = CIRCLE ( 'NONE', #2492, 175.0000000000000000 ) ;
#9002 = CARTESIAN_POINT ( 'NONE',  ( -821.6101090906096260, 83.16704697188406215, -95.16702136683898061 ) ) ;
#9003 = ORIENTED_EDGE ( 'NONE', *, *, #9358, .T. ) ;
#9004 = DIRECTION ( 'NONE',  ( 2.040851148208007875E-17, -1.000000000000000000, -0.000000000000000000 ) ) ;
#9005 = CARTESIAN_POINT ( 'NONE',  ( -1010.922847972426780, 120.6260792194948550, -122.7172756069790296 ) ) ;
#9006 = DIRECTION ( 'NONE',  ( 1.000000000000000000, 0.000000000000000000, -0.000000000000000000 ) ) ;
#9007 = CARTESIAN_POINT ( 'NONE',  ( -127.5000000000000000, 139.9999999999999716, -126.4213562373086575 ) ) ;
#9008 = DIRECTION ( 'NONE',  ( 0.000000000000000000, 0.000000000000000000, -1.000000000000000000 ) ) ;
#9009 = EDGE_LOOP ( 'NONE', ( #45, #7369, #10494, #5898 ) ) ;
#9010 = AXIS2_PLACEMENT_3D ( 'NONE', #9870, #8991, #1580 ) ;
#9011 = ORIENTED_EDGE ( 'NONE', *, *, #11971, .F. ) ;
#9012 = CARTESIAN_POINT ( 'NONE',  ( 19.96273514930160431, 180.6655135177861382, -123.2465523723562910 ) ) ;
#9013 = FACE_BOUND ( 'NONE', #2726, .T. ) ;
#9014 = CARTESIAN_POINT ( 'NONE',  ( -853.5732225365131853, 62.99598188221416706, -154.2940595301278108 ) ) ;
#9015 = CARTESIAN_POINT ( 'NONE',  ( -379.7887390581964837, 100.9343252097582422, -131.1221473163307678 ) ) ;
#9016 = EDGE_CURVE ( 'NONE', #4282, #7284, #1608, .T. ) ;
#9017 = CARTESIAN_POINT ( 'NONE',  ( -374.9550661767995621, 84.88126776701597009, -154.5446018065266287 ) ) ;
#9018 = DIRECTION ( 'NONE',  ( 0.000000000000000000, -1.757987137413040192E-14, 1.000000000000000000 ) ) ;
#9019 = DIRECTION ( 'NONE',  ( 0.000000000000000000, 1.000000000000000000, 0.000000000000000000 ) ) ;
#9020 = CONICAL_SURFACE ( 'NONE', #4297, 9.000000000000000000, 1.047197551196600296 ) ;
#9021 = DIRECTION ( 'NONE',  ( 0.000000000000000000, -1.000000000000000000, 0.000000000000000000 ) ) ;
#9022 = DIRECTION ( 'NONE',  ( -8.163404592832030268E-17, 1.000000000000000000, -0.000000000000000000 ) ) ;
#9023 = ORIENTED_EDGE ( 'NONE', *, *, #10458, .T. ) ;
#9024 = CARTESIAN_POINT ( 'NONE',  ( -956.4793285278399253, 64.87563161486532692, -149.7857175106635452 ) ) ;
#9025 = EDGE_LOOP ( 'NONE', ( #9181, #5254, #8002 ) ) ;
#9026 = AXIS2_PLACEMENT_3D ( 'NONE', #2003, #4837, #2985 ) ;
#9027 = CARTESIAN_POINT ( 'NONE',  ( -19.97946372138042648, 179.5552863838666156, -126.0181968814597582 ) ) ;
#9028 = VERTEX_POINT ( 'NONE', #9342 ) ;
#9029 = ADVANCED_FACE ( 'NONE', ( #8239, #3572, #4394, #1804, #12195 ), #11070, .F. ) ;
#9030 = CARTESIAN_POINT ( 'NONE',  ( -828.5735930359926442, 80.28424781510358343, -94.89227360444822068 ) ) ;
#9031 = DIRECTION ( 'NONE',  ( -0.000000000000000000, 1.000000000000000000, 0.000000000000000000 ) ) ;
#9032 = ORIENTED_EDGE ( 'NONE', *, *, #10153, .F. ) ;
#9033 = CARTESIAN_POINT ( 'NONE',  ( -172.5000000000000000, 151.9999999999999716, -126.4213562373082453 ) ) ;
#9034 = AXIS2_PLACEMENT_3D ( 'NONE', #9585, #3895, #6797 ) ;
#9035 = ORIENTED_EDGE ( 'NONE', *, *, #7129, .T. ) ;
#9036 = CIRCLE ( 'NONE', #5275, 6.500000000000005329 ) ;
#9037 = DIRECTION ( 'NONE',  ( -1.000000000000000000, 0.000000000000000000, 0.000000000000000000 ) ) ;
#9038 = CARTESIAN_POINT ( 'NONE',  ( -87.04832655144203102, 0.000000000000000000, -217.9289243767376831 ) ) ;
#9039 = LINE ( 'NONE', #706, #256 ) ;
#9040 = DIRECTION ( 'NONE',  ( 0.000000000000000000, 0.000000000000000000, -1.000000000000000000 ) ) ;
#9041 = APPLICATION_CONTEXT ( 'automotive_design' ) ;
#9042 = CIRCLE ( 'NONE', #2354, 175.0000000000000000 ) ;
#9043 = CARTESIAN_POINT ( 'NONE',  ( -1015.209561144954137, 93.46821065761379543, -95.06748246948018277 ) ) ;
#9044 = CARTESIAN_POINT ( 'NONE',  ( -37.50000000000000711, 139.9999999999999716, -126.4213562373092685 ) ) ;
#9045 = CARTESIAN_POINT ( 'NONE',  ( -374.8589991914415123, 86.47510645258195439, -95.11294974172253092 ) ) ;
#9046 = CIRCLE ( 'NONE', #10436, 7.500000000000007105 ) ;
#9047 = CARTESIAN_POINT ( 'NONE',  ( 7.500000000000022204, -9.213203435596451385, -126.4213562373094959 ) ) ;
#9048 = CARTESIAN_POINT ( 'NONE',  ( 0.000000000000000000, 0.000000000000000000, 0.000000000000000000 ) ) ;
#9049 = ORIENTED_EDGE ( 'NONE', *, *, #11755, .T. ) ;
#9050 = DIRECTION ( 'NONE',  ( 0.000000000000000000, -0.000000000000000000, 1.000000000000000000 ) ) ;
#9051 = DIRECTION ( 'NONE',  ( 0.000000000000000000, 0.000000000000000000, 1.000000000000000000 ) ) ;
#9052 = DIRECTION ( 'NONE',  ( -0.000000000000000000, 1.000000000000000000, -0.000000000000000000 ) ) ;
#9053 = ORIENTED_EDGE ( 'NONE', *, *, #6462, .F. ) ;
#9054 = CARTESIAN_POINT ( 'NONE',  ( -826.8818560538642259, 82.64726084648152948, -154.2265479354714444 ) ) ;
#9055 = CARTESIAN_POINT ( 'NONE',  ( -927.8303129675875880, 79.95948428978934430, -96.78565065507952170 ) ) ;
#9056 = LINE ( 'NONE', #10177, #5283 ) ;
#9057 = MECHANICAL_DESIGN_GEOMETRIC_PRESENTATION_REPRESENTATION (  '', ( #7493 ), #6894 ) ;
#9058 = CARTESIAN_POINT ( 'NONE',  ( 4.285787411236815022E-15, 24.00000000000001776, -126.4213562373094959 ) ) ;
#9059 = CIRCLE ( 'NONE', #10645, 9.000000000000000000 ) ;
#9060 = FACE_OUTER_BOUND ( 'NONE', #306, .T. ) ;
#9061 = DIRECTION ( 'NONE',  ( 1.000000000000000000, 0.000000000000000000, 0.000000000000000000 ) ) ;
#9062 = CARTESIAN_POINT ( 'NONE',  ( -35.00000000000000000, 11.99999999999999822, 40.70327710424895429 ) ) ;
#9063 = DIRECTION ( 'NONE',  ( -0.000000000000000000, 1.000000000000000000, 7.930164461608263644E-17 ) ) ;
#9064 = CARTESIAN_POINT ( 'NONE',  ( -1028.611899521406940, 50.57492120214474340, -124.6807709998042384 ) ) ;
#9065 = CIRCLE ( 'NONE', #11839, 8.500000000000035527 ) ;
#9066 = FACE_OUTER_BOUND ( 'NONE', #2609, .T. ) ;
#9067 = VERTEX_POINT ( 'NONE', #9147 ) ;
#9068 = CARTESIAN_POINT ( 'NONE',  ( -823.7697810748812799, 117.7733807739867871, -124.6807709998041531 ) ) ;
#9069 = EDGE_CURVE ( 'NONE', #8317, #2603, #4720, .T. ) ;
#9070 = DIRECTION ( 'NONE',  ( -0.000000000000000000, 1.000000000000000000, 0.000000000000000000 ) ) ;
#9071 = DIRECTION ( 'NONE',  ( 0.000000000000000000, 0.000000000000000000, 1.000000000000000000 ) ) ;
#9072 = DIRECTION ( 'NONE',  ( -0.000000000000000000, 1.000000000000000000, -0.000000000000000000 ) ) ;
#9073 = CARTESIAN_POINT ( 'NONE',  ( 20.87244046619806070, 181.4624696265101704, -124.0161187626494126 ) ) ;
#9074 = VERTEX_POINT ( 'NONE', #9214 ) ;
#9075 = CARTESIAN_POINT ( 'NONE',  ( 19.88060343642096583, 180.8815710988893954, -122.4981836151635264 ) ) ;
#9076 = FACE_OUTER_BOUND ( 'NONE', #9937, .T. ) ;
#9077 = FACE_BOUND ( 'NONE', #8226, .T. ) ;
#9078 = CARTESIAN_POINT ( 'NONE',  ( -1065.000000000008868, 82.00000000000028422, -154.8742214401231081 ) ) ;
#9079 = CARTESIAN_POINT ( 'NONE',  ( -824.6569351206132978, 73.74060470499460962, -142.8957018107301451 ) ) ;
#9080 = FILL_AREA_STYLE ('',( #7360 ) ) ;
#9081 = DIRECTION ( 'NONE',  ( 2.040851148208007875E-17, -1.000000000000000000, -0.000000000000000000 ) ) ;
#9082 = CARTESIAN_POINT ( 'NONE',  ( -828.3247893467976155, 76.46300037722042475, -94.69171133721131639 ) ) ;
#9083 = FILL_AREA_STYLE_COLOUR ( '', #10224 ) ;
#9084 = ORIENTED_EDGE ( 'NONE', *, *, #6765, .F. ) ;
#9085 = EDGE_CURVE ( 'NONE', #7650, #5299, #7274, .T. ) ;
#9086 = CARTESIAN_POINT ( 'NONE',  ( -854.0393178910245524, 26.93106345811121827, -136.2353035311989515 ) ) ;
#9087 = EDGE_CURVE ( 'NONE', #559, #12185, #7674, .T. ) ;
#9088 = ORIENTED_EDGE ( 'NONE', *, *, #391, .F. ) ;
#9089 = ORIENTED_EDGE ( 'NONE', *, *, #11969, .F. ) ;
#9090 = CARTESIAN_POINT ( 'NONE',  ( -19.83289927702564626, 180.4664674243214506, -127.2607214279775008 ) ) ;
#9091 = CARTESIAN_POINT ( 'NONE',  ( -144.0488662551579182, 12.00000000000000000, -146.9077238332691877 ) ) ;
#9092 = VERTEX_POINT ( 'NONE', #10629 ) ;
#9093 = CARTESIAN_POINT ( 'NONE',  ( -372.5604626478378805, 62.49331231609644988, -129.1428628536290262 ) ) ;
#9094 = CYLINDRICAL_SURFACE ( 'NONE', #4984, 7.500000000000007105 ) ;
#9095 = ORIENTED_EDGE ( 'NONE', *, *, #7571, .T. ) ;
#9096 = ORIENTED_EDGE ( 'NONE', *, *, #7386, .F. ) ;
#9097 = EDGE_CURVE ( 'NONE', #5849, #9567, #8598, .T. ) ;
#9098 = DIRECTION ( 'NONE',  ( 0.000000000000000000, 0.000000000000000000, -1.000000000000000000 ) ) ;
#9099 = AXIS2_PLACEMENT_3D ( 'NONE', #10501, #4933, #1117 ) ;
#9100 = AXIS2_PLACEMENT_3D ( 'NONE', #7791, #1361, #8834 ) ;
#9101 = EDGE_CURVE ( 'NONE', #11989, #9567, #7874, .T. ) ;
#9102 = DIRECTION ( 'NONE',  ( -8.163404592832031500E-17, 1.000000000000000000, 0.000000000000000000 ) ) ;
#9103 = B_SPLINE_CURVE_WITH_KNOTS ( 'NONE', 3,
 ( #949, #4, #5579, #831, #4604, #11324, #11213, #8376, #12143, #3656, #5639, #896, #7497, #3779, #7555, #2868, #6629, #10392, #8547, #1311, #2232, #2923, #8784, #6685, #8842, #4948, #7677, #8673, #2051, #6930, #10518, #2979, #10461, #5812, #10577, #7619 ),
 .UNSPECIFIED., .F., .F.,
 ( 4, 2, 2, 2, 2, 2, 2, 2, 2, 2, 2, 2, 2, 2, 2, 2, 2, 4 ),
 ( 0.01566607101767062554, 0.01666400919013300008, 0.01766194736259537462, 0.01865988553505774916, 0.01965782370752012370, 0.02065576187998249824, 0.02165370005244487278, 0.02215266913867606352, 0.02265163822490725426, 0.02364957639736996534, 0.02464751456983267641, 0.02564545274229539096, 0.02664339091475809856, 0.02764132908722081311, 0.02863926725968352072, 0.02963720543214623526, 0.03063514360460894634, 0.03163308177707165741 ),
 .UNSPECIFIED. ) ;
#9104 = CARTESIAN_POINT ( 'NONE',  ( -1027.019426772557381, 78.04595964998433999, -95.06748246948046699 ) ) ;
#9105 = CARTESIAN_POINT ( 'NONE',  ( -823.8285638327242850, 78.67432280806536937, -90.68077099980378364 ) ) ;
#9106 = CARTESIAN_POINT ( 'NONE',  ( -27.99999999999999645, -492.9999999999998863, 27.99999999999999645 ) ) ;
#9107 = ADVANCED_FACE ( 'NONE', ( #537 ), #4319, .F. ) ;
#9108 = ADVANCED_FACE ( 'NONE', ( #6118 ), #8093, .F. ) ;
#9109 = AXIS2_PLACEMENT_3D ( 'NONE', #734, #10990, #8288 ) ;
#9110 = ORIENTED_EDGE ( 'NONE', *, *, #5122, .T. ) ;
#9111 = DIRECTION ( 'NONE',  ( 1.186840563529527301E-16, -1.000000000000000000, 0.000000000000000000 ) ) ;
#9112 = LINE ( 'NONE', #6277, #8795 ) ;
#9113 = CARTESIAN_POINT ( 'NONE',  ( 3.123963502971610252E-13, 12.00000000000000000, -96.42135623730949590 ) ) ;
#9114 = ORIENTED_EDGE ( 'NONE', *, *, #7451, .T. ) ;
#9115 = CARTESIAN_POINT ( 'NONE',  ( 7.653191805780027529E-16, 138.9999999999999716, -126.4213562373094959 ) ) ;
#9116 = CARTESIAN_POINT ( 'NONE',  ( -1038.283672687642365, 64.16172732404288581, -96.78565065507946485 ) ) ;
#9117 = DIRECTION ( 'NONE',  ( 0.000000000000000000, 0.000000000000000000, -1.000000000000000000 ) ) ;
#9118 = FACE_OUTER_BOUND ( 'NONE', #1202, .T. ) ;
#9119 = EDGE_CURVE ( 'NONE', #5893, #9384, #4996, .T. ) ;
#9120 = ADVANCED_BREP_SHAPE_REPRESENTATION ( '', ( #12079, #11957 ), #3662 ) ;
#9121 = CARTESIAN_POINT ( 'NONE',  ( 141.4213562373095101, -6.000000000000000000, -1.508194112741312283E-14 ) ) ;
#9122 = CARTESIAN_POINT ( 'NONE',  ( -19.96691528312132036, 179.5908022299374522, -123.3171134976379761 ) ) ;
#9123 = CARTESIAN_POINT ( 'NONE',  ( -141.4213562373095101, -6.000000000000000000, 3.644282033693712520E-14 ) ) ;
#9124 = CARTESIAN_POINT ( 'NONE',  ( -824.4866663711917454, 83.64159454339579725, -104.7481522953014235 ) ) ;
#9125 = CARTESIAN_POINT ( 'NONE',  ( 7.500000000000000000, -5.196152422706638241, -9.000000000000001776 ) ) ;
#9126 = ITEM_DEFINED_TRANSFORMATION ( 'NONE', 'NONE', #1697,  #11957 ) ;
#9127 = VERTEX_POINT ( 'NONE', #11858 ) ;
#9128 = CARTESIAN_POINT ( 'NONE',  ( -126.4213562373094959, 12.00000000000000000, 7.500000000000036415 ) ) ;
#9129 = CARTESIAN_POINT ( 'NONE',  ( -974.1454360724308117, 123.6012932931490127, -118.7903414690677835 ) ) ;
#9130 = CYLINDRICAL_SURFACE ( 'NONE', #5964, 7.500000000000007105 ) ;
#9131 = CARTESIAN_POINT ( 'NONE',  ( -926.6866529579010603, 120.3119365386823034, -141.4553492942759760 ) ) ;
#9132 = CARTESIAN_POINT ( 'NONE',  ( -305.0000000000000568, 151.9999999999999716, -89.68077099980384048 ) ) ;
#9133 = DIRECTION ( 'NONE',  ( -1.000000000000000000, -0.000000000000000000, 0.000000000000000000 ) ) ;
#9134 = CARTESIAN_POINT ( 'NONE',  ( 20.00075211776240991, 181.7166608263125056, -124.5881005502433823 ) ) ;
#9135 = EDGE_LOOP ( 'NONE', ( #11885, #4411 ) ) ;
#9136 = CIRCLE ( 'NONE', #871, 7.500000000000007105 ) ;
#9137 = ORIENTED_EDGE ( 'NONE', *, *, #3666, .T. ) ;
#9138 = CARTESIAN_POINT ( 'NONE',  ( -19.87400029745858987, 179.8933018207857515, -122.4388957686745272 ) ) ;
#9139 = CARTESIAN_POINT ( 'NONE',  ( -379.1619848709565872, 61.99999999999991473, -125.8727444633825883 ) ) ;
#9140 = CARTESIAN_POINT ( 'NONE',  ( -955.6263874535649165, 86.32439835342530898, -154.8742214401227670 ) ) ;
#9141 = CARTESIAN_POINT ( 'NONE',  ( -827.6116022231262832, 75.38889084172119226, -143.5581011396510007 ) ) ;
#9142 = DIRECTION ( 'NONE',  ( 0.000000000000000000, 1.000000000000000000, 0.000000000000000000 ) ) ;
#9143 = DIRECTION ( 'NONE',  ( -0.000000000000000000, 0.000000000000000000, -1.000000000000000000 ) ) ;
#9144 = CARTESIAN_POINT ( 'NONE',  ( -1037.773541645230580, 93.34895244571352180, -152.5758913445289693 ) ) ;
#9145 = DIRECTION ( 'NONE',  ( -0.000000000000000000, 1.000000000000000000, 7.930164461608263644E-17 ) ) ;
#9146 = ORIENTED_EDGE ( 'NONE', *, *, #6406, .F. ) ;
#9147 = CARTESIAN_POINT ( 'NONE',  ( 27.99999999999999645, -6.000000000000000000, 28.00000000000000000 ) ) ;
#9148 = CIRCLE ( 'NONE', #6590, 20.00000000000017053 ) ;
#9149 = ORIENTED_EDGE ( 'NONE', *, *, #8755, .F. ) ;
#9150 = CARTESIAN_POINT ( 'NONE',  ( -928.1401715909056520, 69.16346707077036626, -146.0307792196452965 ) ) ;
#9151 = CARTESIAN_POINT ( 'NONE',  ( 19.84972815362622001, 179.3291729170307462, -127.1285282547103890 ) ) ;
#9152 = EDGE_LOOP ( 'NONE', ( #4365, #6204, #9177, #3445 ) ) ;
#9153 = AXIS2_PLACEMENT_3D ( 'NONE', #12173, #2771, #4564 ) ;
#9154 = ADVANCED_FACE ( 'NONE', ( #7161 ), #5932, .F. ) ;
#9155 = AXIS2_PLACEMENT_3D ( 'NONE', #3211, #3332, #1430 ) ;
#9156 = CARTESIAN_POINT ( 'NONE',  ( -19.98332493385930420, 181.1706761403379744, -125.8191529278201131 ) ) ;
#9157 = DIRECTION ( 'NONE',  ( -0.000000000000000000, 1.000000000000000000, -0.000000000000000000 ) ) ;
#9158 = EDGE_CURVE ( 'NONE', #2533, #10730, #2127, .T. ) ;
#9159 = ORIENTED_EDGE ( 'NONE', *, *, #11803, .F. ) ;
#9160 = CARTESIAN_POINT ( 'NONE',  ( -370.6591228199823718, 57.71959721323136705, -136.2503380851910890 ) ) ;
#9161 = FACE_OUTER_BOUND ( 'NONE', #5004, .T. ) ;
#9162 = ORIENTED_EDGE ( 'NONE', *, *, #1269, .F. ) ;
#9163 = CARTESIAN_POINT ( 'NONE',  ( 1.479627290717497352E-14, -494.9999999999998863, 118.9213562373094817 ) ) ;
#9164 = VERTEX_POINT ( 'NONE', #4197 ) ;
#9165 = CARTESIAN_POINT ( 'NONE',  ( -1048.417899310732537, 40.17786091688628147, -130.5712005305406365 ) ) ;
#9166 = EDGE_CURVE ( 'NONE', #9681, #1855, #6865, .T. ) ;
#9167 = AXIS2_PLACEMENT_3D ( 'NONE', #2168, #4423, #9867 ) ;
#9168 = CIRCLE ( 'NONE', #2658, 7.500000000000012434 ) ;
#9169 = FACE_OUTER_BOUND ( 'NONE', #11181, .T. ) ;
#9170 = CARTESIAN_POINT ( 'NONE',  ( 0.000000000000000000, -7.794228634059935601, 4.500000000000016875 ) ) ;
#9171 = DIRECTION ( 'NONE',  ( 0.000000000000000000, 0.000000000000000000, 1.000000000000000000 ) ) ;
#9172 = CARTESIAN_POINT ( 'NONE',  ( -1038.158164256576356, 71.32123499372119113, -95.06748246948035330 ) ) ;
#9173 = DIRECTION ( 'NONE',  ( 0.000000000000000000, 1.000000000000000000, 0.000000000000000000 ) ) ;
#9174 = DIRECTION ( 'NONE',  ( -1.000000000000000000, 0.000000000000000000, 0.000000000000000000 ) ) ;
#9175 = AXIS2_PLACEMENT_3D ( 'NONE', #11270, #11506, #7731 ) ;
#9176 = CIRCLE ( 'NONE', #288, 7.500000000000007105 ) ;
#9177 = ORIENTED_EDGE ( 'NONE', *, *, #8908, .T. ) ;
#9178 = CARTESIAN_POINT ( 'NONE',  ( -828.8285638327247398, 78.67432280806536937, -158.6807709998041673 ) ) ;
#9179 = EDGE_CURVE ( 'NONE', #5557, #7042, #6465, .T. ) ;
#9180 = CARTESIAN_POINT ( 'NONE',  ( 7.500000000000000000, 5.196152422706624030, -9.000000000000000000 ) ) ;
#9181 = ORIENTED_EDGE ( 'NONE', *, *, #6446, .T. ) ;
#9182 = DIRECTION ( 'NONE',  ( 0.000000000000000000, 0.000000000000000000, -1.000000000000000000 ) ) ;
#9183 = DIRECTION ( 'NONE',  ( -0.05908736525064870598, -0.8481594924192722429, 0.5264353319134452702 ) ) ;
#9184 = CARTESIAN_POINT ( 'NONE',  ( 45.53315400109643463, 0.000000000000000000, -245.3419396193597493 ) ) ;
#9185 = PRODUCT_RELATED_PRODUCT_CATEGORY ( 'part', '', ( #7932 ) ) ;
#9186 = CARTESIAN_POINT ( 'NONE',  ( 0.000000000000000000, 0.000000000000000000, 0.000000000000000000 ) ) ;
#9187 = CIRCLE ( 'NONE', #700, 7.500000000000020428 ) ;
#9188 = FACE_OUTER_BOUND ( 'NONE', #10642, .T. ) ;
#9189 = LINE ( 'NONE', #8212, #11921 ) ;
#9190 = ORIENTED_EDGE ( 'NONE', *, *, #9494, .F. ) ;
#9191 = CARTESIAN_POINT ( 'NONE',  ( -370.3936982783733924, 57.02401252216581184, -133.9834721354013993 ) ) ;
#9192 = ADVANCED_FACE ( 'NONE', ( #1473 ), #9819, .F. ) ;
#9193 = AXIS2_PLACEMENT_3D ( 'NONE', #12219, #783, #5659 ) ;
#9194 = EDGE_LOOP ( 'NONE', ( #6308, #12003, #10309, #325 ) ) ;
#9195 = DIRECTION ( 'NONE',  ( -1.000000000000000000, -1.186840563529527301E-16, 0.000000000000000000 ) ) ;
#9196 = CARTESIAN_POINT ( 'NONE',  ( -1065.000000000003411, 111.6133447792289104, -118.7903414690678972 ) ) ;
#9197 = DIRECTION ( 'NONE',  ( -8.163404592832030268E-17, 1.000000000000000000, -0.000000000000000000 ) ) ;
#9198 = CARTESIAN_POINT ( 'NONE',  ( 2.187692937179487324E-12, 152.0000000000000000, 76.07864376269050410 ) ) ;
#9199 = CARTESIAN_POINT ( 'NONE',  ( -305.0000000000000568, 81.99999999999995737, -89.68077099980384048 ) ) ;
#9200 = CARTESIAN_POINT ( 'NONE',  ( 19.98362395802042712, 181.1895308572829890, -125.8035797126588733 ) ) ;
#9201 = ORIENTED_EDGE ( 'NONE', *, *, #1229, .T. ) ;
#9202 = PRODUCT_DEFINITION_FORMATION_WITH_SPECIFIED_SOURCE ( 'ANY', '', #4767, .NOT_KNOWN. ) ;
#9203 = ORIENTED_EDGE ( 'NONE', *, *, #7970, .F. ) ;
#9204 = AXIS2_PLACEMENT_3D ( 'NONE', #4225, #3399, #10035 ) ;
#9205 = CARTESIAN_POINT ( 'NONE',  ( 126.4213562373094959, -6.000000000000000000, -7.500000000000019540 ) ) ;
#9206 = DIRECTION ( 'NONE',  ( 1.186840563529527301E-16, -1.000000000000000000, 0.000000000000000000 ) ) ;
#9207 = CARTESIAN_POINT ( 'NONE',  ( -1055.782959745576591, 85.17781532426890578, -154.2940595301287203 ) ) ;
#9208 = CARTESIAN_POINT ( 'NONE',  ( -825.1469620822837214, 73.83976809224738247, -142.9404499552406094 ) ) ;
#9209 = DIRECTION ( 'NONE',  ( 0.000000000000000000, 1.000000000000000000, 0.000000000000000000 ) ) ;
#9210 = FACE_OUTER_BOUND ( 'NONE', #4407, .T. ) ;
#9211 = CARTESIAN_POINT ( 'NONE',  ( -853.3345817150077437, 81.97571759610561060, -154.2940595301280098 ) ) ;
#9212 = LINE ( 'NONE', #12059, #3060 ) ;
#9213 = ORIENTED_EDGE ( 'NONE', *, *, #12147, .F. ) ;
#9214 = CARTESIAN_POINT ( 'NONE',  ( -97.49999999999998579, 12.00000000000001421, -126.4213562373088564 ) ) ;
#9215 = VERTEX_POINT ( 'NONE', #3317 ) ;
#9216 = LINE ( 'NONE', #7533, #8043 ) ;
#9217 = CARTESIAN_POINT ( 'NONE',  ( -902.6139906877482417, 77.75433758651681160, -152.5758913445294809 ) ) ;
#9218 = CIRCLE ( 'NONE', #3098, 7.500000000000007105 ) ;
#9219 = VERTEX_POINT ( 'NONE', #4267 ) ;
#9220 = VERTEX_POINT ( 'NONE', #8775 ) ;
#9221 = CARTESIAN_POINT ( 'NONE',  ( -21.06792119228306603, 181.1710195846050340, -126.0693529377697786 ) ) ;
#9222 = LINE ( 'NONE', #2671, #10343 ) ;
#9223 = VERTEX_POINT ( 'NONE', #8035 ) ;
#9224 = AXIS2_PLACEMENT_3D ( 'NONE', #10164, #4549, #7388 ) ;
#9225 = DIRECTION ( 'NONE',  ( -0.000000000000000000, -1.000000000000000000, -0.000000000000000000 ) ) ;
#9226 = CARTESIAN_POINT ( 'NONE',  ( -371.9994406452410090, 61.71775825474107791, -143.7502050151522894 ) ) ;
#9227 = DIRECTION ( 'NONE',  ( -0.000000000000000000, -0.000000000000000000, -1.000000000000000000 ) ) ;
#9228 = DIRECTION ( 'NONE',  ( -1.000000000000000000, -0.000000000000000000, -0.000000000000000000 ) ) ;
#9229 = EDGE_CURVE ( 'NONE', #6316, #5191, #11793, .T. ) ;
#9230 = CARTESIAN_POINT ( 'NONE',  ( -52.49999999999999289, 152.0000000000000000, -126.4213562373090696 ) ) ;
#9231 = AXIS2_PLACEMENT_3D ( 'NONE', #2476, #9022, #1550 ) ;
#9232 = DIRECTION ( 'NONE',  ( 0.000000000000000000, 0.000000000000000000, 1.000000000000000000 ) ) ;
#9233 = CARTESIAN_POINT ( 'NONE',  ( 19.94423941549897705, 178.0993878143254676, -126.1785714357287702 ) ) ;
#9234 = CARTESIAN_POINT ( 'NONE',  ( -853.3345817150102448, 81.97571759610518427, -95.06748246948041015 ) ) ;
#9235 = FACE_OUTER_BOUND ( 'NONE', #942, .T. ) ;
#9236 = CARTESIAN_POINT ( 'NONE',  ( 6.247927005943220505E-13, 164.0000000000000000, -58.92135623730947458 ) ) ;
#9237 = CARTESIAN_POINT ( 'NONE',  ( 154.5043356068769071, 0.000000000000000000, -94.56666130601712439 ) ) ;
#9238 = AXIS2_PLACEMENT_3D ( 'NONE', #1961, #8516, #29 ) ;
#9239 = EDGE_LOOP ( 'NONE', ( #9853, #1090 ) ) ;
#9240 = AXIS2_PLACEMENT_3D ( 'NONE', #8096, #735, #9071 ) ;
#9241 = CARTESIAN_POINT ( 'NONE',  ( 1.874378101782966050E-12, -6.000000000000005329, 53.57864376269050410 ) ) ;
#9242 = DIRECTION ( 'NONE',  ( 0.03251933543158291168, 5.102493419108014449E-16, 0.9994711065474021217 ) ) ;
#9243 = CARTESIAN_POINT ( 'NONE',  ( -7.500000000000007105, 139.9999999999999716, -126.4213562373094959 ) ) ;
#9244 = VERTEX_POINT ( 'NONE', #11801 ) ;
#9245 = DIRECTION ( 'NONE',  ( 0.000000000000000000, 1.000000000000000000, 0.000000000000000000 ) ) ;
#9246 = CARTESIAN_POINT ( 'NONE',  ( -1027.708477481198088, 65.70736702952430619, -99.57582448894528682 ) ) ;
#9247 = CARTESIAN_POINT ( 'NONE',  ( -20.86895858123844860, 178.8871479037923393, -127.0231133604663682 ) ) ;
#9248 = DIRECTION ( 'NONE',  ( -0.000000000000000000, -1.000000000000000000, -0.000000000000000000 ) ) ;
#9249 = EDGE_CURVE ( 'NONE', #11782, #2073, #7099, .T. ) ;
#9250 = VECTOR ( 'NONE', #5943, 1000.000000000000000 ) ;
#9251 = CARTESIAN_POINT ( 'NONE',  ( -824.1700714248495387, 73.67466183167371696, -106.4959216872580186 ) ) ;
#9252 = CARTESIAN_POINT ( 'NONE',  ( -19.95962463553759392, 180.3623627298850067, -123.1966106898677964 ) ) ;
#9253 = CARTESIAN_POINT ( 'NONE',  ( 6.899999999999999467, 5.196152422706624030, -9.000000000000000000 ) ) ;
#9254 = ORIENTED_EDGE ( 'NONE', *, *, #11969, .T. ) ;
#9255 = EDGE_LOOP ( 'NONE', ( #11975, #2987, #8158, #2005 ) ) ;
#9256 = CARTESIAN_POINT ( 'NONE',  ( 4.808665244885994618E-14, -6.000000000000000000, 141.4213562373094817 ) ) ;
#9257 = CARTESIAN_POINT ( 'NONE',  ( -373.5671007695220283, 97.39601910195885637, -111.8308065815015766 ) ) ;
#9258 = AXIS2_PLACEMENT_3D ( 'NONE', #6063, #11575, #5132 ) ;
#9259 = ORIENTED_EDGE ( 'NONE', *, *, #1847, .T. ) ;
#9260 = CARTESIAN_POINT ( 'NONE',  ( 20.00000000000000355, 167.0000000000000000, -124.6807709998038405 ) ) ;
#9261 = CARTESIAN_POINT ( 'NONE',  ( -1037.348432443215870, 116.4729352038311987, -118.7903414690680961 ) ) ;
#9262 = CARTESIAN_POINT ( 'NONE',  ( 21.06240745282767435, 180.3710338094945200, -126.4269926335259129 ) ) ;
#9263 = LINE ( 'NONE', #4639, #10631 ) ;
#9264 = DIRECTION ( 'NONE',  ( -0.000000000000000000, -1.000000000000000000, -0.000000000000000000 ) ) ;
#9265 = ADVANCED_FACE ( 'NONE', ( #3147 ), #9020, .T. ) ;
#9266 = CARTESIAN_POINT ( 'NONE',  ( 21.06786593334110336, 181.1916812352232853, -126.0511736859032936 ) ) ;
#9267 = EDGE_CURVE ( 'NONE', #9219, #10646, #4878, .T. ) ;
#9268 = AXIS2_PLACEMENT_3D ( 'NONE', #11307, #1664, #10315 ) ;
#9269 = ORIENTED_EDGE ( 'NONE', *, *, #5555, .T. ) ;
#9270 = ADVANCED_FACE ( 'NONE', ( #5233 ), #6053, .T. ) ;
#9271 = CIRCLE ( 'NONE', #176, 1.499999999999996447 ) ;
#9272 = DIRECTION ( 'NONE',  ( 0.000000000000000000, 0.000000000000000000, 1.000000000000000000 ) ) ;
#9273 = CARTESIAN_POINT ( 'NONE',  ( 21.06240745282767435, 180.0702511251071485, -126.4269926335259413 ) ) ;
#9274 = CARTESIAN_POINT ( 'NONE',  ( -1031.329434936838197, 101.6864263019769083, -149.7857175106636305 ) ) ;
#9275 = CARTESIAN_POINT ( 'NONE',  ( -369.8922502829638574, 108.2488063532000098, -123.6482589490543376 ) ) ;
#9276 = ADVANCED_FACE ( 'NONE', ( #5055 ), #360, .T. ) ;
#9277 = FILL_AREA_STYLE ('',( #10201 ) ) ;
#9278 = DIRECTION ( 'NONE',  ( 0.000000000000000000, 1.000000000000000000, 0.000000000000000000 ) ) ;
#9279 = LINE ( 'NONE', #817, #2668 ) ;
#9280 = ORIENTED_EDGE ( 'NONE', *, *, #1036, .T. ) ;
#9281 = CARTESIAN_POINT ( 'NONE',  ( -52.49999999999997868, 12.00000000000001421, -126.4213562373090696 ) ) ;
#9282 = LINE ( 'NONE', #10207, #2745 ) ;
#9283 = CARTESIAN_POINT ( 'NONE',  ( -372.4866396559332316, 100.6260255300948501, -145.9099802644697661 ) ) ;
#9284 = ORIENTED_EDGE ( 'NONE', *, *, #2615, .F. ) ;
#9285 = CARTESIAN_POINT ( 'NONE',  ( -927.6556653798983234, 86.18751778479050074, -154.2940595301282656 ) ) ;
#9286 = CARTESIAN_POINT ( 'NONE',  ( 19.99610756949845225, 182.6998913380727743, -125.1317435956655117 ) ) ;
#9287 = ORIENTED_EDGE ( 'NONE', *, *, #8509, .T. ) ;
#9288 = EDGE_CURVE ( 'NONE', #10860, #4714, #2456, .T. ) ;
#9289 = ORIENTED_EDGE ( 'NONE', *, *, #7892, .F. ) ;
#9290 = CARTESIAN_POINT ( 'NONE',  ( -19.98563867331158406, 181.3023397240705776, -125.6985981901809453 ) ) ;
#9291 = DIRECTION ( 'NONE',  ( 0.000000000000000000, 1.000000000000000000, 0.000000000000000000 ) ) ;
#9292 = ORIENTED_EDGE ( 'NONE', *, *, #5688, .T. ) ;
#9293 = CARTESIAN_POINT ( 'NONE',  ( -381.2022825699808664, 65.75744103998614776, -136.3682839401687943 ) ) ;
#9294 = DIRECTION ( 'NONE',  ( 1.000000000000000000, 0.000000000000000000, 0.000000000000000000 ) ) ;
#9295 = APPLICATION_CONTEXT ( 'automotive_design' ) ;
#9296 = PLANE ( 'NONE',  #9026 ) ;
#9297 = ORIENTED_EDGE ( 'NONE', *, *, #10821, .T. ) ;
#9298 = CARTESIAN_POINT ( 'NONE',  ( 27.99999999999999645, -492.9999999999998863, 27.99999999999999645 ) ) ;
#9299 = CARTESIAN_POINT ( 'NONE',  ( 7.500000000000000000, 10.39230484541327115, -2.602085213965207092E-15 ) ) ;
#9300 = CARTESIAN_POINT ( 'NONE',  ( -1019.723937646958007, 86.79129919622097589, -94.48732055948626396 ) ) ;
#9301 = DIRECTION ( 'NONE',  ( -0.000000000000000000, -1.000000000000000000, -1.757987137413040192E-14 ) ) ;
#9302 = CARTESIAN_POINT ( 'NONE',  ( -270.0000000000000000, 12.00000000000001066, -126.4213562373076059 ) ) ;
#9303 = CARTESIAN_POINT ( 'NONE',  ( -1063.013736978594579, 47.55218547899811199, -126.6442663926291914 ) ) ;
#9304 = CARTESIAN_POINT ( 'NONE',  ( -820.4056028115179515, 82.32260517263534894, -144.6785023965176435 ) ) ;
#9305 = ORIENTED_EDGE ( 'NONE', *, *, #11520, .F. ) ;
#9306 = CARTESIAN_POINT ( 'NONE',  ( -826.0529305544605450, 83.16438776978687031, -144.6472496521799371 ) ) ;
#9307 = DIRECTION ( 'NONE',  ( 0.3483833211657269557, -1.994778970785637675E-17, -0.9373521544934636518 ) ) ;
#9308 = CARTESIAN_POINT ( 'NONE',  ( -370.4017534246571586, 106.9526614274764853, -115.3486010405474929 ) ) ;
#9309 = EDGE_LOOP ( 'NONE', ( #827, #8666 ) ) ;
#9310 = DIRECTION ( 'NONE',  ( 0.000000000000000000, 0.000000000000000000, 1.000000000000000000 ) ) ;
#9311 = CARTESIAN_POINT ( 'NONE',  ( -1057.299536696272526, 52.76571712355550403, -103.3307627799637487 ) ) ;
#9312 = DIRECTION ( 'NONE',  ( -0.000000000000000000, -1.000000000000000000, -0.000000000000000000 ) ) ;
#9313 = DIRECTION ( 'NONE',  ( -1.000000000000000000, 0.000000000000000000, 0.000000000000000000 ) ) ;
#9314 = CARTESIAN_POINT ( 'NONE',  ( 21.06569119078285013, 179.6122972493173222, -126.3061156060180963 ) ) ;
#9315 = FACE_OUTER_BOUND ( 'NONE', #1239, .T. ) ;
#9316 = CARTESIAN_POINT ( 'NONE',  ( -19.03136272649511085, 180.2041921146316668, -134.6807709998038547 ) ) ;
#9317 = CARTESIAN_POINT ( 'NONE',  ( -19.98204207764186791, 179.1370916267982523, -123.6234561704243475 ) ) ;
#9318 = CARTESIAN_POINT ( 'NONE',  ( -828.5731535248124828, 77.06390383656750487, -144.0645491675084884 ) ) ;
#9319 = VECTOR ( 'NONE', #3190, 1000.000000000000000 ) ;
#9320 = EDGE_CURVE ( 'NONE', #6696, #9788, #1734, .T. ) ;
#9321 = EDGE_LOOP ( 'NONE', ( #11834, #322 ) ) ;
#9322 = CARTESIAN_POINT ( 'NONE',  ( 126.4213562373094959, -494.9999999999998863, -7.500000000000019540 ) ) ;
#9323 = ITEM_DEFINED_TRANSFORMATION ( 'NONE', 'NONE', #2288,  #11957 ) ;
#9324 = CARTESIAN_POINT ( 'NONE',  ( -383.9019967062238834, 90.88042285000165066, -106.7131948037297349 ) ) ;
#9325 = ADVANCED_FACE ( 'NONE', ( #10416 ), #7453, .T. ) ;
#9326 = ORIENTED_EDGE ( 'NONE', *, *, #8523, .T. ) ;
#9327 = CARTESIAN_POINT ( 'NONE',  ( 19.88538568419372154, 178.7282225113628726, -126.8218319435565604 ) ) ;
#9328 = VECTOR ( 'NONE', #7166, 1000.000000000000000 ) ;
#9329 = ADVANCED_FACE ( 'NONE', ( #602 ), #5414, .F. ) ;
#9330 = CARTESIAN_POINT ( 'NONE',  ( 21.06533532366276162, 180.7746266989912272, -126.3260595342268715 ) ) ;
#9331 = ORIENTED_EDGE ( 'NONE', *, *, #11060, .T. ) ;
#9332 = ORIENTED_EDGE ( 'NONE', *, *, #11879, .F. ) ;
#9333 = CARTESIAN_POINT ( 'NONE',  ( -1024.691966601152672, 118.8493250655916142, -124.6807709998039400 ) ) ;
#9334 = LINE ( 'NONE', #10130, #1432 ) ;
#9335 = DIRECTION ( 'NONE',  ( -1.000000000000000000, 0.000000000000000000, 0.000000000000000000 ) ) ;
#9336 = CARTESIAN_POINT ( 'NONE',  ( -1061.276350651670782, 98.40484402385492047, -149.7857175106635452 ) ) ;
#9337 = PRESENTATION_STYLE_ASSIGNMENT (( #5562 ) ) ;
#9338 = CARTESIAN_POINT ( 'NONE',  ( -27.99999999999999645, -492.9999999999998863, -27.99999999999999645 ) ) ;
#9339 = CARTESIAN_POINT ( 'NONE',  ( -1031.476138302183244, 95.34216976508434982, -152.5758913445290830 ) ) ;
#9340 = EDGE_CURVE ( 'NONE', #11012, #4868, #4442, .T. ) ;
#9341 = ORIENTED_EDGE ( 'NONE', *, *, #4405, .F. ) ;
#9342 = CARTESIAN_POINT ( 'NONE',  ( 29.95840947131252108, 180.2041921146317520, -138.2654117679341539 ) ) ;
#9343 = ADVANCED_FACE ( 'NONE', ( #1728, #2576 ), #5486, .F. ) ;
#9344 = ORIENTED_EDGE ( 'NONE', *, *, #9652, .T. ) ;
#9345 = CARTESIAN_POINT ( 'NONE',  ( -1012.527716518106786, 86.38194213450564973, -154.8742214401233070 ) ) ;
#9346 = CIRCLE ( 'NONE', #1848, 7.500000000000007105 ) ;
#9347 = EDGE_LOOP ( 'NONE', ( #11469, #1997, #10305, #7556 ) ) ;
#9348 = PRODUCT_DEFINITION ( 'UNKNOWN', '', #6834, #2087 ) ;
#9349 = ORIENTED_EDGE ( 'NONE', *, *, #2065, .F. ) ;
#9350 = CARTESIAN_POINT ( 'NONE',  ( -828.7978644797699417, 79.31746325908761719, -144.5027040960659974 ) ) ;
#9351 = CARTESIAN_POINT ( 'NONE',  ( -19.99699311396506118, 181.6109172643918157, -124.1290590095319430 ) ) ;
#9352 = CARTESIAN_POINT ( 'NONE',  ( -1038.595419435783924, 46.89684673038589580, -141.4553492942758623 ) ) ;
#9353 = AXIS2_PLACEMENT_3D ( 'NONE', #7460, #3610, #9313 ) ;
#9354 = ORIENTED_EDGE ( 'NONE', *, *, #4745, .F. ) ;
#9355 = CARTESIAN_POINT ( 'NONE',  ( -372.7850951469527558, 63.30985991596471507, -132.0026127303325438 ) ) ;
#9356 = DIRECTION ( 'NONE',  ( 0.000000000000000000, 0.000000000000000000, -1.000000000000000000 ) ) ;
#9358 = EDGE_CURVE ( 'NONE', #8251, #9588, #12181, .T. ) ;
#9357 = FACE_OUTER_BOUND ( 'NONE', #2776, .T. ) ;
#9359 = CARTESIAN_POINT ( 'NONE',  ( 35.00000000000000000, 152.0000000000000000, 190.3192290001959748 ) ) ;
#9360 = AXIS2_PLACEMENT_3D ( 'NONE', #981, #4302, #7076 ) ;
#9361 = AXIS2_PLACEMENT_3D ( 'NONE', #3385, #555, #9894 ) ;
#9362 = LINE ( 'NONE', #5391, #2113 ) ;
#9363 = DIRECTION ( 'NONE',  ( 0.000000000000000000, 0.000000000000000000, -1.000000000000000000 ) ) ;
#9364 = AXIS2_PLACEMENT_3D ( 'NONE', #9577, #5857, #167 ) ;
#9365 = CARTESIAN_POINT ( 'NONE',  ( -956.7203770923135835, 58.97922774997691420, -103.3307627799636919 ) ) ;
#9366 = CARTESIAN_POINT ( 'NONE',  ( -29.99999999999998579, -9.213203435596451385, -126.4213562373092685 ) ) ;
#9367 = DIRECTION ( 'NONE',  ( -1.224646799147353207E-16, -1.453460497224676649E-32, 1.000000000000000000 ) ) ;
#9368 = CARTESIAN_POINT ( 'NONE',  ( -928.4368846968627622, 59.55532739646334051, -122.7172756069790154 ) ) ;
#9369 = VERTEX_POINT ( 'NONE', #731 ) ;
#9370 = CIRCLE ( 'NONE', #8776, 1.000000000000000888 ) ;
#9371 = CARTESIAN_POINT ( 'NONE',  ( -818.8285638327206470, 78.67432280806529832, -144.4023295390026931 ) ) ;
#9372 = AXIS2_PLACEMENT_3D ( 'NONE', #3619, #665, #8283 ) ;
#9373 = VECTOR ( 'NONE', #11836, 1000.000000000000000 ) ;
#9374 = CARTESIAN_POINT ( 'NONE',  ( -371.1191838156116773, 105.0141530621877166, -110.0650553684051403 ) ) ;
#9375 = ORIENTED_EDGE ( 'NONE', *, *, #1269, .T. ) ;
#9376 = CARTESIAN_POINT ( 'NONE',  ( -1038.595419435790973, 46.89684673038605922, -107.9061927053327850 ) ) ;
#9377 = LINE ( 'NONE', #11475, #1356 ) ;
#9378 = CARTESIAN_POINT ( 'NONE',  ( -27.99999999999999645, -492.9999999999998863, 27.99999999999999645 ) ) ;
#9379 = CARTESIAN_POINT ( 'NONE',  ( 19.97857452415077972, 179.6604161890264493, -126.0626113202902587 ) ) ;
#9380 = AXIS2_PLACEMENT_3D ( 'NONE', #2253, #5026, #5088 ) ;
#9381 = AXIS2_PLACEMENT_3D ( 'NONE', #9199, #2890, #12115 ) ;
#9382 = DIRECTION ( 'NONE',  ( 0.7071067811865479058, -0.000000000000000000, 0.7071067811865472397 ) ) ;
#9383 = CARTESIAN_POINT ( 'NONE',  ( -19.99961582769660140, 178.6962453788212031, -124.8244425039453915 ) ) ;
#9384 = VERTEX_POINT ( 'NONE', #8348 ) ;
#9385 = DIRECTION ( 'NONE',  ( 0.7071067811865473507, 0.000000000000000000, -0.7071067811865477948 ) ) ;
#9386 = ITEM_DEFINED_TRANSFORMATION ( 'NONE', 'NONE', #10186,  #11957 ) ;
#9387 = CARTESIAN_POINT ( 'NONE',  ( -374.7973491424790495, 88.50727265276420042, -105.6931112893597771 ) ) ;
#9388 = VERTEX_POINT ( 'NONE', #6291 ) ;
#9389 = CARTESIAN_POINT ( 'NONE',  ( -1031.000617048998265, 115.3267894020684992, -113.1262384684098521 ) ) ;
#9390 = AXIS2_PLACEMENT_3D ( 'NONE', #9180, #12024, #3539 ) ;
#9391 = CARTESIAN_POINT ( 'NONE',  ( 120.8820948793965186, 0.000000000000000000, -179.1989091883332890 ) ) ;
#9392 = EDGE_CURVE ( 'NONE', #1835, #10209, #10060, .T. ) ;
#9393 = EDGE_CURVE ( 'NONE', #8852, #11444, #7827, .T. ) ;
#9394 = VERTEX_POINT ( 'NONE', #6348 ) ;
#9395 = VERTEX_POINT ( 'NONE', #3622 ) ;
#9396 = CARTESIAN_POINT ( 'NONE',  ( -954.0441199534440102, 124.9954171138387977, -124.6807709998039115 ) ) ;
#9397 = LINE ( 'NONE', #933, #6695 ) ;
#9398 = CARTESIAN_POINT ( 'NONE',  ( -37.50000000000000000, 24.00000000000001421, -126.4213562373092685 ) ) ;
#9399 = CARTESIAN_POINT ( 'NONE',  ( -955.3297122972861644, 93.84065249268903131, -154.2940595301280950 ) ) ;
#9400 = FACE_OUTER_BOUND ( 'NONE', #4303, .T. ) ;
#9401 = DIRECTION ( 'NONE',  ( 0.000000000000000000, 0.000000000000000000, 1.000000000000000000 ) ) ;
#9402 = CARTESIAN_POINT ( 'NONE',  ( -1023.078931369431530, 98.73915068298377662, -152.5758913445292535 ) ) ;
#9403 = CARTESIAN_POINT ( 'NONE',  ( -151.3258811035894098, 12.00000000000000000, -63.63263083939681053 ) ) ;
#9404 = VERTEX_POINT ( 'NONE', #9128 ) ;
#9405 = CARTESIAN_POINT ( 'NONE',  ( -373.4654644648271073, 97.87726989067260774, -136.9400350704844129 ) ) ;
#9406 = ORIENTED_EDGE ( 'NONE', *, *, #4346, .F. ) ;
#9407 = CARTESIAN_POINT ( 'NONE',  ( -820.4595805503685142, 72.64106675864371709, -154.8742214401225397 ) ) ;
#9408 = EDGE_CURVE ( 'NONE', #1622, #7207, #3466, .T. ) ;
#9409 = ORIENTED_EDGE ( 'NONE', *, *, #4727, .T. ) ;
#9410 = AXIS2_PLACEMENT_3D ( 'NONE', #2986, #11516, #2124 ) ;
#9411 = VERTEX_POINT ( 'NONE', #11980 ) ;
#9412 = EDGE_CURVE ( 'NONE', #2975, #4344, #9993, .T. ) ;
#9413 = DIRECTION ( 'NONE',  ( 0.000000000000000000, 1.000000000000000000, 0.000000000000000000 ) ) ;
#9414 = DIRECTION ( 'NONE',  ( 2.040851148208007875E-17, -1.000000000000000000, -0.000000000000000000 ) ) ;
#9415 = CARTESIAN_POINT ( 'NONE',  ( -1016.863910020547223, 59.13213530333427315, -141.4553492942757487 ) ) ;
#9416 = VERTEX_POINT ( 'NONE', #9789 ) ;
#9417 = CARTESIAN_POINT ( 'NONE',  ( -384.1670479773604256, 74.31760017581927968, -143.1493696165661333 ) ) ;
#9418 = DIRECTION ( 'NONE',  ( 0.000000000000000000, 0.000000000000000000, -1.000000000000000000 ) ) ;
#9419 = CARTESIAN_POINT ( 'NONE',  ( -372.8161565995750948, 64.64827838876098554, -102.1643297174437635 ) ) ;
#9420 = CYLINDRICAL_SURFACE ( 'NONE', #6666, 7.500000000000007105 ) ;
#9421 = EDGE_CURVE ( 'NONE', #7650, #1611, #9974, .T. ) ;
#9422 = DIRECTION ( 'NONE',  ( 0.000000000000000000, 1.000000000000000000, 0.000000000000000000 ) ) ;
#9423 = DIRECTION ( 'NONE',  ( 0.9501779778103252028, 0.000000000000000000, 0.3117078928809489669 ) ) ;
#9424 = AXIS2_PLACEMENT_3D ( 'NONE', #7134, #6148, #582 ) ;
#9425 = EDGE_CURVE ( 'NONE', #569, #822, #11970, .T. ) ;
#9426 = CARTESIAN_POINT ( 'NONE',  ( -1062.493403002516516, 61.99900353997416147, -99.57582448894515892 ) ) ;
#9427 = CARTESIAN_POINT ( 'NONE',  ( -825.4402961394322347, 83.41886444745711060, -104.7307635270716304 ) ) ;
#9428 = FACE_OUTER_BOUND ( 'NONE', #2796, .T. ) ;
#9429 = CARTESIAN_POINT ( 'NONE',  ( -1048.417899310732537, 40.17786091688628147, -130.5712005305406365 ) ) ;
#9430 = B_SPLINE_CURVE_WITH_KNOTS ( 'NONE', 3,
 ( #8958, #4153, #9017, #7868, #11697, #11641, #3159, #488, #10699, #3210, #10759, #9830, #2409, #8894, #419, #4209, #7986, #11759, #7045, #4277, #8046, #11815, #3331, #7110, #10874, #5244 ),
 .UNSPECIFIED., .F., .F.,
 ( 4, 2, 2, 2, 2, 2, 2, 2, 2, 2, 2, 2, 4 ),
 ( 0.1348585005367443912, 0.1392389232406545940, 0.1414291345926096954, 0.1425242402685872323, 0.1436193459445647691, 0.1479997686484748332, 0.1501899800004299068, 0.1523801913523849527, 0.1567606140562951278, 0.1589508254082501737, 0.1611410367602052196, 0.1655214594641153114, 0.1699018821680253755 ),
 .UNSPECIFIED. ) ;
#9431 = ORIENTED_EDGE ( 'NONE', *, *, #93, .F. ) ;
#9432 = CARTESIAN_POINT ( 'NONE',  ( -828.7978644797661900, 79.31746325908696349, -144.5027040960656564 ) ) ;
#9433 = CARTESIAN_POINT ( 'NONE',  ( 126.4213562373095385, -485.4999999999998863, -6.938893903907228378E-15 ) ) ;
#9434 = ORIENTED_EDGE ( 'NONE', *, *, #3959, .T. ) ;
#9435 = DIRECTION ( 'NONE',  ( 0.000000000000000000, -1.156482317317870246E-16, 1.000000000000000000 ) ) ;
#9436 = CARTESIAN_POINT ( 'NONE',  ( -927.9936929689729368, 74.21188826700399943, -99.57582448894522997 ) ) ;
#9437 = CIRCLE ( 'NONE', #4703, 7.500000000000020428 ) ;
#9438 = DIRECTION ( 'NONE',  ( 1.000000000000000000, 0.000000000000000000, 0.000000000000000000 ) ) ;
#9439 = CARTESIAN_POINT ( 'NONE',  ( -217.5000000000000000, -9.213203435596478030, -126.4213562373080180 ) ) ;
#9440 = DIRECTION ( 'NONE',  ( -1.876626137810916309E-30, -1.000000000000000000, -4.930380657631307143E-31 ) ) ;
#9441 = CARTESIAN_POINT ( 'NONE',  ( -19.98084489187587565, 177.8063731767314266, -125.5691280742910436 ) ) ;
#9442 = CYLINDRICAL_SURFACE ( 'NONE', #4822, 7.500000000000007105 ) ;
#9443 = CIRCLE ( 'NONE', #10816, 134.9999999999999716 ) ;
#9444 = ORIENTED_EDGE ( 'NONE', *, *, #401, .F. ) ;
#9445 = CYLINDRICAL_SURFACE ( 'NONE', #9360, 7.500000000000007105 ) ;
#9446 = CARTESIAN_POINT ( 'NONE',  ( -373.6858788323772842, 95.50525450785576709, -98.95117123207425891 ) ) ;
#9447 = EDGE_LOOP ( 'NONE', ( #7743, #5161, #4163, #3347 ) ) ;
#9448 = VECTOR ( 'NONE', #8571, 1000.000000000000000 ) ;
#9449 = DIRECTION ( 'NONE',  ( -1.000000000000000000, 0.000000000000000000, 0.000000000000000000 ) ) ;
#9450 = CARTESIAN_POINT ( 'NONE',  ( 21.02276486677203593, 181.6974666944221042, -125.0994992711609370 ) ) ;
#9451 = FACE_BOUND ( 'NONE', #6334, .T. ) ;
#9452 = VERTEX_POINT ( 'NONE', #7379 ) ;
#9453 = DIRECTION ( 'NONE',  ( -1.000000000000000000, 0.000000000000000000, 0.000000000000000000 ) ) ;
#9454 =( REPRESENTATION_RELATIONSHIP ('NONE','NONE', #12149, #690 ) REPRESENTATION_RELATIONSHIP_WITH_TRANSFORMATION ( #9126 )SHAPE_REPRESENTATION_RELATIONSHIP( ) );
#9455 = DIRECTION ( 'NONE',  ( 0.000000000000000000, 1.000000000000000000, 0.000000000000000000 ) ) ;
#9456 = FACE_OUTER_BOUND ( 'NONE', #4970, .T. ) ;
#9457 = CARTESIAN_POINT ( 'NONE',  ( -822.2439855206093853, 97.57287547056431265, -149.7857175106634600 ) ) ;
#9458 = EDGE_CURVE ( 'NONE', #3054, #10902, #6577, .T. ) ;
#9459 = LINE ( 'NONE', #2040, #5016 ) ;
#9460 = ORIENTED_EDGE ( 'NONE', *, *, #3602, .F. ) ;
#9461 = FACE_OUTER_BOUND ( 'NONE', #3169, .T. ) ;
#9462 = ORIENTED_EDGE ( 'NONE', *, *, #9087, .F. ) ;
#9463 = CIRCLE ( 'NONE', #11038, 7.500000000000007994 ) ;
#9464 = FACE_BOUND ( 'NONE', #5692, .T. ) ;
#9465 = ORIENTED_EDGE ( 'NONE', *, *, #6820, .F. ) ;
#9466 = DIRECTION ( 'NONE',  ( 0.3117078928809249860, -1.670400663243698742E-14, 0.9501779778103330854 ) ) ;
#9467 = ORIENTED_EDGE ( 'NONE', *, *, #504, .F. ) ;
#9468 = CARTESIAN_POINT ( 'NONE',  ( -828.3910170805090729, 80.72627522873344219, -144.6407408995351318 ) ) ;
#9469 = CARTESIAN_POINT ( 'NONE',  ( -19.98203294318189549, 182.6106388860948471, -125.5411158980709558 ) ) ;
#9470 = DIRECTION ( 'NONE',  ( -8.163404592832030268E-17, 1.000000000000000000, -0.000000000000000000 ) ) ;
#9471 = CARTESIAN_POINT ( 'NONE',  ( -997.4616017999776432, 44.34671234275830187, -141.4553492942759476 ) ) ;
#9472 = VERTEX_POINT ( 'NONE', #3663 ) ;
#9473 = ADVANCED_FACE ( 'NONE', ( #5450 ), #11085, .F. ) ;
#9474 = CARTESIAN_POINT ( 'NONE',  ( -374.9351506289129361, 85.78662242748217182, -144.3442421662540198 ) ) ;
#9475 = DIRECTION ( 'NONE',  ( 0.000000000000000000, -1.156482317317870246E-16, 1.000000000000000000 ) ) ;
#9476 = CARTESIAN_POINT ( 'NONE',  ( -374.2976682315979247, 70.77949302303818513, -108.0449445377915225 ) ) ;
#9477 = AXIS2_PLACEMENT_3D ( 'NONE', #1042, #3069, #7645 ) ;
#9478 = EDGE_CURVE ( 'NONE', #10836, #3679, #9796, .T. ) ;
#9479 = EDGE_CURVE ( 'NONE', #5900, #11808, #2488, .T. ) ;
#9480 = DIRECTION ( 'NONE',  ( -0.000000000000000000, 1.000000000000000000, -0.000000000000000000 ) ) ;
#9481 = DIRECTION ( 'NONE',  ( -8.163404592832030268E-17, 1.000000000000000000, -0.000000000000000000 ) ) ;
#9482 = CARTESIAN_POINT ( 'NONE',  ( -67.49999999999998579, -9.213203435596451385, -126.4213562373090696 ) ) ;
#9483 = CARTESIAN_POINT ( 'NONE',  ( -818.6751755801135459, 47.70925804672316417, -99.57582448894514471 ) ) ;
#9484 = DIRECTION ( 'NONE',  ( 0.000000000000000000, 1.000000000000000000, 0.000000000000000000 ) ) ;
#9485 = CARTESIAN_POINT ( 'NONE',  ( -1028.611899521407167, 50.57492120214475761, -126.6442663926292340 ) ) ;
#9486 = ORIENTED_EDGE ( 'NONE', *, *, #544, .F. ) ;
#9487 = ORIENTED_EDGE ( 'NONE', *, *, #4178, .F. ) ;
#9488 = CARTESIAN_POINT ( 'NONE',  ( -820.5266942580627756, 82.43260598963586006, -144.6763645173219004 ) ) ;
#9489 = SHAPE_DEFINITION_REPRESENTATION ( #10493, #2032 ) ;
#9490 = CARTESIAN_POINT ( 'NONE',  ( -141.4213562373095101, -492.9999999999998863, 3.644282033693712520E-14 ) ) ;
#9491 = ADVANCED_FACE ( 'NONE', ( #4038 ), #11579, .T. ) ;
#9492 = ORIENTED_EDGE ( 'NONE', *, *, #10686, .F. ) ;
#9493 = CARTESIAN_POINT ( 'NONE',  ( -795.0000000000050022, 56.89504896194521422, -107.9061927053325860 ) ) ;
#9494 = EDGE_CURVE ( 'NONE', #9074, #966, #7629, .T. ) ;
#9495 = CARTESIAN_POINT ( 'NONE',  ( -6.106226635438360972E-13, 12.00000000000000000, -252.1807709998039115 ) ) ;
#9496 = DIRECTION ( 'NONE',  ( -1.000000000000000000, 0.000000000000000000, 0.000000000000000000 ) ) ;
#9497 = CARTESIAN_POINT ( 'NONE',  ( 126.4213562373094959, 0.000000000000000000, -7.500000000000020428 ) ) ;
#9498 = CARTESIAN_POINT ( 'NONE',  ( 19.84263310680793069, 179.5276748199284214, -127.1852985703725807 ) ) ;
#9499 = EDGE_CURVE ( 'NONE', #10559, #5214, #10648, .T. ) ;
#9500 = DIRECTION ( 'NONE',  ( 0.000000000000000000, 1.000000000000000000, -0.000000000000000000 ) ) ;
#9501 = ORIENTED_EDGE ( 'NONE', *, *, #6600, .T. ) ;
#9502 = PRODUCT_DEFINITION_SHAPE ( 'NONE', 'NONE',  #10256 ) ;
#9503 = FACE_OUTER_BOUND ( 'NONE', #8429, .T. ) ;
#9504 = CARTESIAN_POINT ( 'NONE',  ( -374.5716219028437308, 90.99737113659554666, -106.7529307625888606 ) ) ;
#9505 = ORIENTED_EDGE ( 'NONE', *, *, #4369, .T. ) ;
#9506 = CARTESIAN_POINT ( 'NONE',  ( -992.1517139731023462, 115.6613254010895986, -107.9061927053323870 ) ) ;
#9507 = EDGE_CURVE ( 'NONE', #8317, #5359, #6819, .T. ) ;
#9508 = CARTESIAN_POINT ( 'NONE',  ( -1021.913416468810851, 116.8879375517085464, -136.2353035311978431 ) ) ;
#9509 = CARTESIAN_POINT ( 'NONE',  ( 19.98133380395517378, 177.8015904785984560, -125.5720248138883193 ) ) ;
#9510 = AXIS2_PLACEMENT_3D ( 'NONE', #4146, #3204, #5128 ) ;
#9511 = CARTESIAN_POINT ( 'NONE',  ( -904.2101318205999405, 125.2895275102983419, -124.6807709998041531 ) ) ;
#9512 = ORIENTED_EDGE ( 'NONE', *, *, #6889, .F. ) ;
#9513 = DIRECTION ( 'NONE',  ( 0.000000000000000000, 1.000000000000000000, 6.938893903907169213E-16 ) ) ;
#9514 = CARTESIAN_POINT ( 'NONE',  ( -144.0488662551579182, 12.00000000000000000, -154.4077238332691877 ) ) ;
#9515 = DIRECTION ( 'NONE',  ( 0.000000000000000000, 5.522905491341382306E-16, 1.000000000000000000 ) ) ;
#9516 = CARTESIAN_POINT ( 'NONE',  ( -992.5689194452182846, 110.2481211102048491, -146.0307792196443870 ) ) ;
#9517 = CARTESIAN_POINT ( 'NONE',  ( 1.734723475976807094E-15, 180.2041921146324910, -179.7948474705909234 ) ) ;
#9518 = DIRECTION ( 'NONE',  ( -1.000000000000000000, -1.186840563529527301E-16, 0.000000000000000000 ) ) ;
#9519 = EDGE_LOOP ( 'NONE', ( #1301, #3305 ) ) ;
#9520 = VECTOR ( 'NONE', #7614, 1000.000000000000000 ) ;
#9521 = CARTESIAN_POINT ( 'NONE',  ( -373.2951768170237301, 97.35898663981262757, -149.0144453010688039 ) ) ;
#9522 = CARTESIAN_POINT ( 'NONE',  ( -954.7734463792789938, 107.7731650919854758, -149.7857175106632042 ) ) ;
#9523 = DIRECTION ( 'NONE',  ( 0.000000000000000000, 0.000000000000000000, 1.000000000000000000 ) ) ;
#9524 = ORIENTED_EDGE ( 'NONE', *, *, #9777, .T. ) ;
#9525 = EDGE_LOOP ( 'NONE', ( #2160, #1849, #10536, #2897 ) ) ;
#9526 = AXIS2_PLACEMENT_3D ( 'NONE', #5198, #9031, #572 ) ;
#9527 = CARTESIAN_POINT ( 'NONE',  ( -120.0000000000000000, 139.9999999999999716, -126.4213562373086575 ) ) ;
#9528 = CARTESIAN_POINT ( 'NONE',  ( -20.00099490938537627, 182.7248142053001629, -124.9210440959558355 ) ) ;
#9529 = FACE_OUTER_BOUND ( 'NONE', #6738, .T. ) ;
#9530 = CARTESIAN_POINT ( 'NONE',  ( -1057.299536696276846, 52.76571712355565325, -146.0307792196449554 ) ) ;
#9531 = ORIENTED_EDGE ( 'NONE', *, *, #3118, .F. ) ;
#9532 = CARTESIAN_POINT ( 'NONE',  ( -373.4691676486093570, 67.36345505517621746, -149.6605093826277084 ) ) ;
#9533 = DIRECTION ( 'NONE',  ( -8.163404592832031500E-17, 1.000000000000000000, 0.000000000000000000 ) ) ;
#9534 = CARTESIAN_POINT ( 'NONE',  ( -382.5041789709763407, 68.77964067713233476, -109.6698101448797615 ) ) ;
#9535 = FILL_AREA_STYLE ('',( #5759 ) ) ;
#9536 = CARTESIAN_POINT ( 'NONE',  ( -957.1839320239870403, 48.17551948191491817, -130.5712005305400112 ) ) ;
#9537 = ORIENTED_EDGE ( 'NONE', *, *, #4514, .F. ) ;
#9538 = ADVANCED_FACE ( 'NONE', ( #10526 ), #10589, .F. ) ;
#9539 = EDGE_LOOP ( 'NONE', ( #2575, #518 ) ) ;
#9540 = EDGE_CURVE ( 'NONE', #1863, #8366, #1087, .T. ) ;
#9541 = AXIS2_PLACEMENT_3D ( 'NONE', #4626, #3543, #4432 ) ;
#9542 = CARTESIAN_POINT ( 'NONE',  ( -953.5758047008322364, 72.53746257253780527, -96.78565065507940801 ) ) ;
#9543 = CARTESIAN_POINT ( 'NONE',  ( -827.8090925714953983, 81.71768170412181576, -104.6809152895179693 ) ) ;
#9544 = CARTESIAN_POINT ( 'NONE',  ( -997.9925905826634107, 37.72784750336339954, -130.5712005305403238 ) ) ;
#9545 = ORIENTED_EDGE ( 'NONE', *, *, #10982, .F. ) ;
#9546 = CARTESIAN_POINT ( 'NONE',  ( -974.2138504089066373, 120.9496320545085695, -136.2353035311977010 ) ) ;
#9547 = ORIENTED_EDGE ( 'NONE', *, *, #2590, .F. ) ;
#9548 = EDGE_CURVE ( 'NONE', #481, #9741, #7430, .T. ) ;
#9549 = APPLICATION_PROTOCOL_DEFINITION ( 'draft international standard', 'automotive_design', 1998, #4235 ) ;
#9550 = ORIENTED_EDGE ( 'NONE', *, *, #5385, .F. ) ;
#9551 = CARTESIAN_POINT ( 'NONE',  ( -1038.664246639915291, 43.28664065472965206, -113.1262384684093405 ) ) ;
#9552 = AXIS2_PLACEMENT_3D ( 'NONE', #6217, #585, #8816 ) ;
#9553 = DIRECTION ( 'NONE',  ( 2.040851148208007875E-17, -1.000000000000000000, -0.000000000000000000 ) ) ;
#9554 = VECTOR ( 'NONE', #3909, 1000.000000000000000 ) ;
#9555 = DIRECTION ( 'NONE',  ( -1.000000000000000000, 0.000000000000000000, 0.000000000000000000 ) ) ;
#9556 = DIRECTION ( 'NONE',  ( -1.186840563529527301E-16, 1.000000000000000000, -0.000000000000000000 ) ) ;
#9557 = CARTESIAN_POINT ( 'NONE',  ( -992.1517139731023462, 115.6613254010895986, -107.9061927053323870 ) ) ;
#9558 = FACE_BOUND ( 'NONE', #1157, .T. ) ;
#9559 = CARTESIAN_POINT ( 'NONE',  ( -21.05708315573553691, 178.8782276755749194, -125.6123305554640837 ) ) ;
#9560 = DIRECTION ( 'NONE',  ( 0.000000000000000000, 0.000000000000000000, 1.000000000000000000 ) ) ;
#9561 = AXIS2_PLACEMENT_3D ( 'NONE', #1877, #5514, #8315 ) ;
#9562 = ADVANCED_FACE ( 'NONE', ( #2935 ), #7812, .T. ) ;
#9563 = AXIS2_PLACEMENT_3D ( 'NONE', #5503, #6249, #5367 ) ;
#9564 = ORIENTED_EDGE ( 'NONE', *, *, #9392, .F. ) ;
#9565 = AXIS2_PLACEMENT_3D ( 'NONE', #4117, #5841, #5777 ) ;
#9566 = CARTESIAN_POINT ( 'NONE',  ( -375.0000000000000000, 81.43281243045049678, -154.6807709998038263 ) ) ;
#9567 = VERTEX_POINT ( 'NONE', #2007 ) ;
#9568 = CARTESIAN_POINT ( 'NONE',  ( -852.8684863605125202, 118.0406360202081970, -113.1262384684093405 ) ) ;
#9569 = CARTESIAN_POINT ( 'NONE',  ( -1037.348432443219735, 116.4729352038311987, -130.5712005305406080 ) ) ;
#9570 = CARTESIAN_POINT ( 'NONE',  ( 4.335549520754014653E-15, 167.0000000000000000, -124.6807709998038405 ) ) ;
#9571 = AXIS2_PLACEMENT_3D ( 'NONE', #3953, #1861, #4017 ) ;
#9572 = CARTESIAN_POINT ( 'NONE',  ( -795.0000000000046612, 112.0000000000007532, -122.7172756069791717 ) ) ;
#9573 = VERTEX_POINT ( 'NONE', #4960 ) ;
#9574 = FACE_OUTER_BOUND ( 'NONE', #5130, .T. ) ;
#9575 = ADVANCED_FACE ( 'NONE', ( #254 ), #4787, .F. ) ;
#9576 = CARTESIAN_POINT ( 'NONE',  ( -374.5762240358420740, 89.76870905692126712, -95.99562579782801208 ) ) ;
#9577 = CARTESIAN_POINT ( 'NONE',  ( -823.8285638327245124, 78.67432280806536937, -159.6807709998044800 ) ) ;
#9578 = PLANE ( 'NONE',  #2153 ) ;
#9579 = CARTESIAN_POINT ( 'NONE',  ( -904.0006525278439540, 119.6095687608908378, -141.4553492942759760 ) ) ;
#9580 = CARTESIAN_POINT ( 'NONE',  ( -370.0786918602308333, 107.7875646358821200, -118.7374980023263049 ) ) ;
#9581 = AXIS2_PLACEMENT_3D ( 'NONE', #6828, #6947, #10533 ) ;
#9582 =( NAMED_UNIT ( * ) PLANE_ANGLE_UNIT ( ) SI_UNIT ( $, .RADIAN. ) );
#9583 = CARTESIAN_POINT ( 'NONE',  ( -19.99999999999999645, 177.7115707886035807, -124.6807709997916334 ) ) ;
#9584 = ORIENTED_EDGE ( 'NONE', *, *, #7454, .F. ) ;
#9585 = CARTESIAN_POINT ( 'NONE',  ( 45.53315400109643463, 12.00000000000000000, -237.8419396193597208 ) ) ;
#9586 = CARTESIAN_POINT ( 'NONE',  ( -992.1517139731079169, 115.6613254010897123, -141.4553492942762318 ) ) ;
#9587 = CARTESIAN_POINT ( 'NONE',  ( 1.387778780781445676E-14, -494.9999999999998863, 133.9213562373095101 ) ) ;
#9588 = VERTEX_POINT ( 'NONE', #8684 ) ;
#9589 = CIRCLE ( 'NONE', #8419, 8.999999999999998224 ) ;
#9590 = ORIENTED_EDGE ( 'NONE', *, *, #3405, .T. ) ;
#9591 = DIRECTION ( 'NONE',  ( 0.000000000000000000, 0.000000000000000000, 1.000000000000000000 ) ) ;
#9592 = CARTESIAN_POINT ( 'NONE',  ( -1028.007066121607295, 60.50166182213178701, -146.0307792196450123 ) ) ;
#9593 = ORIENTED_EDGE ( 'NONE', *, *, #3755, .T. ) ;
#9594 = CARTESIAN_POINT ( 'NONE',  ( -374.8301963407180892, 76.83280000780887065, -154.1603600426035428 ) ) ;
#9595 = FACE_OUTER_BOUND ( 'NONE', #10173, .T. ) ;
#9596 = CARTESIAN_POINT ( 'NONE',  ( -374.0135547283281312, 68.94350272267550395, -109.4340150406342218 ) ) ;
#9597 = SURFACE_SIDE_STYLE ('',( #10763 ) ) ;
#9598 = AXIS2_PLACEMENT_3D ( 'NONE', #310, #417, #6808 ) ;
#9599 = ORIENTED_EDGE ( 'NONE', *, *, #1026, .T. ) ;
#9600 = CARTESIAN_POINT ( 'NONE',  ( 6.899999999999999467, 0.000000000000000000, 0.000000000000000000 ) ) ;
#9601 = ORIENTED_EDGE ( 'NONE', *, *, #2463, .F. ) ;
#9602 = PRODUCT_DEFINITION_SHAPE ( 'NONE', 'NONE',  #12240 ) ;
#9603 = DIRECTION ( 'NONE',  ( -0.000000000000000000, 0.000000000000000000, -1.000000000000000000 ) ) ;
#9604 = VECTOR ( 'NONE', #5408, 1000.000000000000000 ) ;
#9605 = CARTESIAN_POINT ( 'NONE',  ( -1038.506348936316726, 51.71309463382168303, -103.3307627799636350 ) ) ;
#9606 = CARTESIAN_POINT ( 'NONE',  ( -825.1278902672622735, 83.51360356663572304, -104.7380248171176618 ) ) ;
#9607 = ORIENTED_EDGE ( 'NONE', *, *, #3216, .T. ) ;
#9608 = CIRCLE ( 'NONE', #4284, 7.500000000000020428 ) ;
#9609 = CARTESIAN_POINT ( 'NONE',  ( -826.3315746005818028, 74.34282231245687456, -154.6710292045187032 ) ) ;
#9610 = EDGE_LOOP ( 'NONE', ( #11490, #2207 ) ) ;
#9611 = EDGE_CURVE ( 'NONE', #9730, #140, #3977, .T. ) ;
#9612 = ORIENTED_EDGE ( 'NONE', *, *, #5019, .T. ) ;
#9613 = CARTESIAN_POINT ( 'NONE',  ( -1032.644706488208840, 45.21923725197571997, -118.7903414690683519 ) ) ;
#9614 = LINE ( 'NONE', #8464, #5690 ) ;
#9615 = DIRECTION ( 'NONE',  ( 1.000000000000000000, 0.000000000000000000, 0.000000000000000000 ) ) ;
#9616 = CARTESIAN_POINT ( 'NONE',  ( 35.00000000000000000, 152.0000000000000000, -124.6807709998038689 ) ) ;
#9617 = CIRCLE ( 'NONE', #4091, 7.500000000000007994 ) ;
#9618 = DIRECTION ( 'NONE',  ( -1.000000000000000000, 0.000000000000000000, 0.000000000000000000 ) ) ;
#9619 = CARTESIAN_POINT ( 'NONE',  ( -21.06782237318494211, 179.3291273983845429, -126.1426500519474416 ) ) ;
#9620 = ORIENTED_EDGE ( 'NONE', *, *, #5034, .F. ) ;
#9621 = AXIS2_PLACEMENT_3D ( 'NONE', #9105, #5590, #710 ) ;
#9622 = ORIENTED_EDGE ( 'NONE', *, *, #10982, .T. ) ;
#9624 = EDGE_CURVE ( 'NONE', #11206, #4244, #6643, .T. ) ;
#9623 = CARTESIAN_POINT ( 'NONE',  ( -1014.632462699974781, 105.5176738732103132, -99.57582448894522997 ) ) ;
#9625 = CARTESIAN_POINT ( 'NONE',  ( -974.1454360724337675, 123.6012932931491690, -130.5712005305403238 ) ) ;
#9626 = CARTESIAN_POINT ( 'NONE',  ( 4.335549520754014653E-15, 167.0000000000000000, -124.6807709998038405 ) ) ;
#9627 = EDGE_CURVE ( 'NONE', #1702, #4714, #7232, .T. ) ;
#9629 = B_SPLINE_CURVE_WITH_KNOTS ( 'NONE', 3,
 ( #1023, #5710, #1089, #3736, #1948, #8559 ),
 .UNSPECIFIED., .F., .F.,
 ( 4, 2, 4 ),
 ( 2.380730970505090229E-07, 0.002629065763328472353, 0.005257893453559894098 ),
 .UNSPECIFIED. ) ;
#9628 = CARTESIAN_POINT ( 'NONE',  ( -852.8175266017511831, 121.6828083272127685, -124.6807709998041247 ) ) ;
#9630 = ORIENTED_EDGE ( 'NONE', *, *, #8556, .F. ) ;
#9631 = CARTESIAN_POINT ( 'NONE',  ( -126.4213562373094959, 12.00000000000000000, 2.255140518769849223E-14 ) ) ;
#9632 = DIRECTION ( 'NONE',  ( 0.000000000000000000, 0.000000000000000000, 1.000000000000000000 ) ) ;
#9633 = CARTESIAN_POINT ( 'NONE',  ( -217.5000000000000000, 139.9999999999999716, -126.4213562373080180 ) ) ;
#9634 = CARTESIAN_POINT ( 'NONE',  ( -795.0000000000046612, 103.3499740386315864, -146.0307792196441312 ) ) ;
#9635 = CARTESIAN_POINT ( 'NONE',  ( -380.2012603716702870, 100.1962551005152733, -116.3549404919051113 ) ) ;
#9636 = DIRECTION ( 'NONE',  ( 0.000000000000000000, 0.000000000000000000, 1.000000000000000000 ) ) ;
#9637 = VECTOR ( 'NONE', #7960, 1000.000000000000000 ) ;
#9638 = DIRECTION ( 'NONE',  ( -8.163404592832030268E-17, 1.000000000000000000, -0.000000000000000000 ) ) ;
#9639 =( NAMED_UNIT ( * ) PLANE_ANGLE_UNIT ( ) SI_UNIT ( $, .RADIAN. ) );
#9640 = EDGE_LOOP ( 'NONE', ( #8966, #4295 ) ) ;
#9641 = CARTESIAN_POINT ( 'NONE',  ( 1.479627290717497352E-14, -492.9999999999998863, 118.9213562373094817 ) ) ;
#9642 = AXIS2_PLACEMENT_3D ( 'NONE', #10191, #12114, #5674 ) ;
#9643 = CARTESIAN_POINT ( 'NONE',  ( -1011.418100375194967, 110.6663390795549162, -146.0307792196444723 ) ) ;
#9644 = EDGE_CURVE ( 'NONE', #8525, #1654, #11188, .T. ) ;
#9645 = EDGE_CURVE ( 'NONE', #5463, #11262, #5077, .T. ) ;
#9646 = CARTESIAN_POINT ( 'NONE',  ( -180.0000000000000000, 139.9999999999999716, -126.4213562373082453 ) ) ;
#9647 = EDGE_LOOP ( 'NONE', ( #6375, #1109, #11556, #9305 ) ) ;
#9648 = VECTOR ( 'NONE', #10741, 1000.000000000000000 ) ;
#9649 = ORIENTED_EDGE ( 'NONE', *, *, #4133, .F. ) ;
#9650 = CARTESIAN_POINT ( 'NONE',  ( 19.99153366631225381, 178.9186500652280642, -123.8934111528711668 ) ) ;
#9651 = AXIS2_PLACEMENT_3D ( 'NONE', #10077, #11999, #11134 ) ;
#9652 = EDGE_CURVE ( 'NONE', #10209, #2073, #4475, .T. ) ;
#9653 = EDGE_CURVE ( 'NONE', #6215, #2282, #10980, .T. ) ;
#9654 = CARTESIAN_POINT ( 'NONE',  ( -379.7887390581964837, 100.9343252097582564, -131.1221473163307678 ) ) ;
#9655 = CARTESIAN_POINT ( 'NONE',  ( -1065.000000000007731, 60.65002596136951496, -146.0307792196448986 ) ) ;
#9656 = LINE ( 'NONE', #8728, #5832 ) ;
#9657 = CARTESIAN_POINT ( 'NONE',  ( -384.9995590721709959, 82.68011010844932684, -144.6800286746663460 ) ) ;
#9658 = DIRECTION ( 'NONE',  ( 0.000000000000000000, 0.000000000000000000, -1.000000000000000000 ) ) ;
#9659 = CARTESIAN_POINT ( 'NONE',  ( -384.4111993152493483, 75.51142861137186912, -105.7511216177616120 ) ) ;
#9660 = SURFACE_STYLE_USAGE ( .BOTH. , #9597 ) ;
#9661 = COLOUR_RGB ( '', 0.72549020, 0.75294118, 0.79215686) ;
#9662 = ORIENTED_EDGE ( 'NONE', *, *, #2693, .T. ) ;
#9663 = EDGE_CURVE ( 'NONE', #2064, #1499, #9964, .T. ) ;
#9664 = EDGE_LOOP ( 'NONE', ( #631, #1773, #8588, #1247 ) ) ;
#9665 = DIRECTION ( 'NONE',  ( -0.000000000000000000, -1.000000000000000000, -0.000000000000000000 ) ) ;
#9666 = CARTESIAN_POINT ( 'NONE',  ( -1025.943122242217214, 53.12767954719360830, -118.7903414690682524 ) ) ;
#9667 = AXIS2_PLACEMENT_3D ( 'NONE', #6409, #1584, #1647 ) ;
#9668 = CARTESIAN_POINT ( 'NONE',  ( -19.92945081678884023, 182.1752604789721488, -126.3669219011512297 ) ) ;
#9669 = CARTESIAN_POINT ( 'NONE',  ( -1021.483947769362658, 56.15424078096121008, -136.2353035311990368 ) ) ;
#9670 = VERTEX_POINT ( 'NONE', #9841 ) ;
#9671 = CARTESIAN_POINT ( 'NONE',  ( -384.7236254841880623, 86.46752657155295196, -105.1769125859564014 ) ) ;
#9672 = CARTESIAN_POINT ( 'NONE',  ( -825.1261283413638239, 73.83457159616112619, -154.6564883458196107 ) ) ;
#9673 = ORIENTED_EDGE ( 'NONE', *, *, #5229, .F. ) ;
#9674 = CARTESIAN_POINT ( 'NONE',  ( 151.3258811035896656, 12.00000000000000000, -56.13263083939798292 ) ) ;
#9675 = ORIENTED_EDGE ( 'NONE', *, *, #68, .F. ) ;
#9676 = CARTESIAN_POINT ( 'NONE',  ( -1048.417899310738221, 40.17786091688638095, -118.7903414690680250 ) ) ;
#9677 = FACE_OUTER_BOUND ( 'NONE', #10393, .T. ) ;
#9678 = FACE_BOUND ( 'NONE', #11435, .T. ) ;
#9679 = CARTESIAN_POINT ( 'NONE',  ( -1037.656130532294128, 99.96792753513312846, -99.57582448894522997 ) ) ;
#9680 = CARTESIAN_POINT ( 'NONE',  ( -19.98933286486646210, 178.9475762002984709, -125.5057985845799635 ) ) ;
#9681 = VERTEX_POINT ( 'NONE', #5258 ) ;
#9682 = DIRECTION ( 'NONE',  ( 0.000000000000000000, 5.522905491341382306E-16, 1.000000000000000000 ) ) ;
#9683 = ORIENTED_EDGE ( 'NONE', *, *, #5555, .F. ) ;
#9684 = CARTESIAN_POINT ( 'NONE',  ( -1046.676250823070177, 92.10743237175765330, -96.78565065507946485 ) ) ;
#9685 = EDGE_LOOP ( 'NONE', ( #591, #10390 ) ) ;
#9686 = CARTESIAN_POINT ( 'NONE',  ( -87.04832655144203102, 12.00000000000000000, -210.4289243767376831 ) ) ;
#9687 = CARTESIAN_POINT ( 'NONE',  ( -28.53314250459844459, 180.2041921146317236, -137.7978499286130898 ) ) ;
#9688 = EDGE_CURVE ( 'NONE', #3344, #7569, #5655, .T. ) ;
#9689 = CARTESIAN_POINT ( 'NONE',  ( -954.0441199534440102, 124.9954171138387977, -124.6807709998039115 ) ) ;
#9690 = ORIENTED_EDGE ( 'NONE', *, *, #4645, .F. ) ;
#9691 = CARTESIAN_POINT ( 'NONE',  ( -151.3258811035894098, 0.000000000000000000, -56.13263083939680342 ) ) ;
#9692 = ADVANCED_FACE ( 'NONE', ( #565 ), #4345, .F. ) ;
#9693 = CARTESIAN_POINT ( 'NONE',  ( 9.381075359908434252E-13, 164.0000000000000000, -43.92135623730948879 ) ) ;
#9694 = CARTESIAN_POINT ( 'NONE',  ( -818.8285638327242850, 78.67432280806571043, -264.6807709998050200 ) ) ;
#9695 = CARTESIAN_POINT ( 'NONE',  ( -1014.007272717915953, 117.9006809476442896, -136.2353035311982126 ) ) ;
#9696 = AXIS2_PLACEMENT_3D ( 'NONE', #3535, #7199, #2495 ) ;
#9697 = LINE ( 'NONE', #1238, #5822 ) ;
#9698 = ORIENTED_EDGE ( 'NONE', *, *, #6443, .F. ) ;
#9699 = FACE_OUTER_BOUND ( 'NONE', #7752, .T. ) ;
#9700 = CARTESIAN_POINT ( 'NONE',  ( -180.0000000000000000, 24.00000000000001421, -126.4213562373082453 ) ) ;
#9701 = FACE_OUTER_BOUND ( 'NONE', #12065, .T. ) ;
#9702 = EDGE_CURVE ( 'NONE', #7767, #1233, #7033, .T. ) ;
#9703 = PRODUCT_DEFINITION_SHAPE ( 'NONE', 'NONE',  #12248 ) ;
#9704 = FACE_OUTER_BOUND ( 'NONE', #1057, .T. ) ;
#9705 = CARTESIAN_POINT ( 'NONE',  ( -1061.104375862961888, 103.3839434440459968, -146.0307792196447565 ) ) ;
#9706 = AXIS2_PLACEMENT_3D ( 'NONE', #8825, #5224, #2389 ) ;
#9707 = CARTESIAN_POINT ( 'NONE',  ( 6.247927005943220505E-13, 152.0000000000000000, -58.92135623730947458 ) ) ;
#9708 = ORIENTED_EDGE ( 'NONE', *, *, #11442, .F. ) ;
#9709 = CARTESIAN_POINT ( 'NONE',  ( -270.0000000000000000, -9.213203435596478030, -126.4213562373076059 ) ) ;
#9710 = VERTEX_POINT ( 'NONE', #8980 ) ;
#9711 = CARTESIAN_POINT ( 'NONE',  ( 20.78030879612743931, 179.3744110069277724, -123.5640671919478280 ) ) ;
#9712 = CARTESIAN_POINT ( 'NONE',  ( -384.4692968731354199, 88.15998365774518675, -143.7178510142985886 ) ) ;
#9713 = CARTESIAN_POINT ( 'NONE',  ( -1013.392840968502924, 67.31954129910421614, -149.7857175106636873 ) ) ;
#9714 = CIRCLE ( 'NONE', #6362, 7.500000000000020428 ) ;
#9715 = ADVANCED_FACE ( 'NONE', ( #7948 ), #510, .F. ) ;
#9716 = CARTESIAN_POINT ( 'NONE',  ( -240.0000000000000000, 24.00000000000000711, -126.4213562373078190 ) ) ;
#9717 = CARTESIAN_POINT ( 'NONE',  ( 0.000000000000000000, 0.000000000000000000, -126.4213562373094959 ) ) ;
#9718 = SURFACE_SIDE_STYLE ('',( #5136 ) ) ;
#9719 = AXIS2_PLACEMENT_3D ( 'NONE', #11258, #11125, #2650 ) ;
#9720 = AXIS2_PLACEMENT_3D ( 'NONE', #7004, #11651, #10715 ) ;
#9721 = ORIENTED_EDGE ( 'NONE', *, *, #7087, .T. ) ;
#9722 = CARTESIAN_POINT ( 'NONE',  ( -976.2351830775012331, 35.86345807843999012, -118.7903414690679824 ) ) ;
#9723 = CARTESIAN_POINT ( 'NONE',  ( -19.94418321653721549, 182.3098040923358951, -126.1872098885080646 ) ) ;
#9724 = ORIENTED_EDGE ( 'NONE', *, *, #1929, .T. ) ;
#9725 = EDGE_CURVE ( 'NONE', #12174, #9411, #3395, .T. ) ;
#9726 = CARTESIAN_POINT ( 'NONE',  ( -825.8938804283657191, 83.23078805786300904, -95.20686423277604149 ) ) ;
#9727 = VERTEX_POINT ( 'NONE', #10897 ) ;
#9728 = CARTESIAN_POINT ( 'NONE',  ( -820.5243268950206357, 74.90756738765448119, -154.6705515957940520 ) ) ;
#9729 = AXIS2_PLACEMENT_3D ( 'NONE', #3783, #8501, #2000 ) ;
#9730 = VERTEX_POINT ( 'NONE', #7012 ) ;
#9731 = ITEM_DEFINED_TRANSFORMATION ( 'NONE', 'NONE', #7625,  #11957 ) ;
#9732 = VERTEX_POINT ( 'NONE', #10841 ) ;
#9733 = CARTESIAN_POINT ( 'NONE',  ( -854.0902776497799778, 23.28889115110665742, -122.7172756069793138 ) ) ;
#9734 = CARTESIAN_POINT ( 'NONE',  ( 0.000000000000000000, -494.9999999999998863, -118.9213562373094817 ) ) ;
#9735 = VECTOR ( 'NONE', #3489, 1000.000000000000000 ) ;
#9736 = CARTESIAN_POINT ( 'NONE',  ( -795.0000000000002274, 98.77454568802498613, -99.57582448894500260 ) ) ;
#9737 = LINE ( 'NONE', #583, #213 ) ;
#9738 = ORIENTED_EDGE ( 'NONE', *, *, #913, .F. ) ;
#9739 = CARTESIAN_POINT ( 'NONE',  ( 2.186774452080127126E-12, -6.000000000000005329, 83.57864376269050410 ) ) ;
#9740 = CIRCLE ( 'NONE', #7382, 7.500000000000007105 ) ;
#9741 = VERTEX_POINT ( 'NONE', #441 ) ;
#9742 = CARTESIAN_POINT ( 'NONE',  ( -821.6815100408621220, 89.78153722040228502, -96.78565065507908116 ) ) ;
#9743 = ORIENTED_EDGE ( 'NONE', *, *, #10751, .F. ) ;
#9744 = CARTESIAN_POINT ( 'NONE',  ( -852.8684863605087685, 118.0406360202081970, -136.2353035311977862 ) ) ;
#9745 = CARTESIAN_POINT ( 'NONE',  ( 2.186774452080127126E-12, 152.0000000000000000, 91.07864376269051832 ) ) ;
#9746 = DIRECTION ( 'NONE',  ( -0.000000000000000000, 1.000000000000000000, 7.930164461608263644E-17 ) ) ;
#9747 = CIRCLE ( 'NONE', #11733, 7.500000000000007105 ) ;
#9748 = AXIS2_PLACEMENT_3D ( 'NONE', #10135, #4588, #8364 ) ;
#9749 = CARTESIAN_POINT ( 'NONE',  ( 126.4213562373094959, 12.00000000000000000, -7.500000000000020428 ) ) ;
#9750 = CARTESIAN_POINT ( 'NONE',  ( 4.454233577106967753E-15, 166.0000000000000000, -124.6807709998038405 ) ) ;
#9751 = FACE_OUTER_BOUND ( 'NONE', #10599, .T. ) ;
#9752 = CYLINDRICAL_SURFACE ( 'NONE', #11027, 7.500000000000012434 ) ;
#9753 = DIRECTION ( 'NONE',  ( -0.000000000000000000, -0.000000000000000000, 1.000000000000000000 ) ) ;
#9754 = DIRECTION ( 'NONE',  ( 0.000000000000000000, -1.000000000000000000, 0.000000000000000000 ) ) ;
#9755 = ORIENTED_EDGE ( 'NONE', *, *, #4070, .F. ) ;
#9756 = DIRECTION ( 'NONE',  ( 0.000000000000000000, 0.000000000000000000, 1.000000000000000000 ) ) ;
#9757 = AXIS2_PLACEMENT_3D ( 'NONE', #6428, #7298, #1665 ) ;
#9758 = DIRECTION ( 'NONE',  ( -1.000000000000000000, 0.000000000000000000, 0.000000000000000000 ) ) ;
#9759 = EDGE_CURVE ( 'NONE', #11886, #4553, #3278, .T. ) ;
#9760 = AXIS2_PLACEMENT_3D ( 'NONE', #1451, #8201, #8987 ) ;
#9761 = CARTESIAN_POINT ( 'NONE',  ( 144.0488662551573782, 0.000000000000000000, -139.4077238332702109 ) ) ;
#9762 = EDGE_CURVE ( 'NONE', #7569, #3344, #9608, .T. ) ;
#9763 = CARTESIAN_POINT ( 'NONE',  ( 9.381075359908434252E-13, -6.000000000000004441, -43.92135623730950300 ) ) ;
#9764 = ORIENTED_EDGE ( 'NONE', *, *, #9854, .T. ) ;
#9765 = ORIENTED_EDGE ( 'NONE', *, *, #11081, .T. ) ;
#9766 = CARTESIAN_POINT ( 'NONE',  ( 20.73051967732101630, 180.6106195048880068, -123.3499684708650506 ) ) ;
#9767 = AXIS2_PLACEMENT_3D ( 'NONE', #2562, #9052, #3200 ) ;
#9768 = CIRCLE ( 'NONE', #4839, 0.5999999999999998668 ) ;
#9769 = FACE_BOUND ( 'NONE', #6868, .T. ) ;
#9770 = CARTESIAN_POINT ( 'NONE',  ( -1016.123300349502756, 74.17810748283176281, -152.5758913445294525 ) ) ;
#9771 = DIRECTION ( 'NONE',  ( 0.000000000000000000, 0.000000000000000000, -1.000000000000000000 ) ) ;
#9772 = FACE_OUTER_BOUND ( 'NONE', #2373, .T. ) ;
#9773 = CARTESIAN_POINT ( 'NONE',  ( 35.00000000000000000, 81.99999999999998579, 190.3192290001959748 ) ) ;
#9774 = DIRECTION ( 'NONE',  ( 0.000000000000000000, 1.000000000000000000, 0.000000000000000000 ) ) ;
#9775 = DIRECTION ( 'NONE',  ( 3.061276722312011504E-17, -1.000000000000000000, 0.000000000000000000 ) ) ;
#9776 = VERTEX_POINT ( 'NONE', #1389 ) ;
#9777 = EDGE_CURVE ( 'NONE', #4285, #64, #2429, .T. ) ;
#9778 = STYLED_ITEM ( 'NONE', ( #280 ), #11906 ) ;
#9779 = EDGE_LOOP ( 'NONE', ( #6869, #11216, #6644, #10222 ) ) ;
#9780 = EDGE_CURVE ( 'NONE', #6370, #7586, #4274, .T. ) ;
#9781 = CARTESIAN_POINT ( 'NONE',  ( -1028.611899521406713, 50.57492120214472919, -122.7172756069792428 ) ) ;
#9782 = DIRECTION ( 'NONE',  ( -0.000000000000000000, 0.000000000000000000, -1.000000000000000000 ) ) ;
#9783 = CARTESIAN_POINT ( 'NONE',  ( -19.89470248115624074, 181.2369511437511278, -122.6240768797811853 ) ) ;
#9784 = CARTESIAN_POINT ( 'NONE',  ( -828.3149917726251488, 80.88765617246495765, -94.94636425413492020 ) ) ;
#9785 = AXIS2_PLACEMENT_3D ( 'NONE', #4208, #4031, #1428 ) ;
#9786 = DIRECTION ( 'NONE',  ( -8.163404592832030268E-17, 1.000000000000000000, -0.000000000000000000 ) ) ;
#9787 = DIRECTION ( 'NONE',  ( 0.000000000000000000, 0.000000000000000000, 1.000000000000000000 ) ) ;
#9788 = VERTEX_POINT ( 'NONE', #7894 ) ;
#9789 = CARTESIAN_POINT ( 'NONE',  ( 7.500000000000030198, -6.999999999999977796, -124.6807709998038405 ) ) ;
#9790 = ORIENTED_EDGE ( 'NONE', *, *, #11514, .F. ) ;
#9791 = CARTESIAN_POINT ( 'NONE',  ( -1038.719578313837474, 40.52245044769760085, -126.6442663926297740 ) ) ;
#9792 = DIRECTION ( 'NONE',  ( -1.186840563529527301E-16, 1.000000000000000000, -0.000000000000000000 ) ) ;
#9793 = EDGE_CURVE ( 'NONE', #4581, #3571, #4233, .T. ) ;
#9794 = ADVANCED_FACE ( 'NONE', ( #1507 ), #3404, .F. ) ;
#9795 = UNCERTAINTY_MEASURE_WITH_UNIT (LENGTH_MEASURE( 1.000000000000000082E-05 ), #4176, 'distance_accuracy_value', 'NONE');
#9796 = CIRCLE ( 'NONE', #9410, 7.500000000000007105 ) ;
#9797 = CARTESIAN_POINT ( 'NONE',  ( -795.0000000000070486, 103.3499740386316859, -103.3307627799634218 ) ) ;
#9798 = CARTESIAN_POINT ( 'NONE',  ( -172.5000000000000000, 12.00000000000001421, -126.4213562373082453 ) ) ;
#9799 = ORIENTED_EDGE ( 'NONE', *, *, #11954, .T. ) ;
#9800 = PRODUCT_DEFINITION_SHAPE ( 'NONE', 'NONE',  #191 ) ;
#9801 = DIRECTION ( 'NONE',  ( -1.186840563529527301E-16, 1.000000000000000000, -0.000000000000000000 ) ) ;
#9802 = CARTESIAN_POINT ( 'NONE',  ( -374.6679438209018826, 88.82298366188321381, -95.70765607985160273 ) ) ;
#9803 = ORIENTED_EDGE ( 'NONE', *, *, #7038, .T. ) ;
#9804 = CARTESIAN_POINT ( 'NONE',  ( -821.0802431487063586, 81.36881375820571805, -95.06748246948008330 ) ) ;
#9805 = AXIS2_PLACEMENT_3D ( 'NONE', #11169, #1774, #786 ) ;
#9806 = CARTESIAN_POINT ( 'NONE',  ( 4.454233577106967753E-15, 166.0000000000000000, -124.6807709998038405 ) ) ;
#9807 = CARTESIAN_POINT ( 'NONE',  ( -1060.756016675586807, 112.8516620848305934, -124.6807709998040821 ) ) ;
#9808 = DIRECTION ( 'NONE',  ( 3.061276722312011504E-17, -1.000000000000000000, -0.000000000000000000 ) ) ;
#9809 = CARTESIAN_POINT ( 'NONE',  ( -35.00000000000000000, 2.428612866367529932E-14, -159.6807709998040252 ) ) ;
#9810 = CARTESIAN_POINT ( 'NONE',  ( -1030.944970944895431, 117.4714819019837222, -118.7903414690680535 ) ) ;
#9811 = DIRECTION ( 'NONE',  ( -0.9501779778103373042, 0.000000000000000000, 0.3117078928809121074 ) ) ;
#9812 = CARTESIAN_POINT ( 'NONE',  ( -19.91081574664456610, 181.5182364730087272, -122.7941294590837913 ) ) ;
#9813 = TOROIDAL_SURFACE ( 'NONE', #11217, 6.599999999999998757, 0.5999999999999999778 ) ;
#9814 = FACE_BOUND ( 'NONE', #4582, .T. ) ;
#9815 = CARTESIAN_POINT ( 'NONE',  ( -379.5936447076720697, 62.72305949846725071, -119.2434292096965720 ) ) ;
#9816 = CARTESIAN_POINT ( 'NONE',  ( 0.000000000000000000, 164.0000000000000000, -126.4213562373094959 ) ) ;
#9817 = DIRECTION ( 'NONE',  ( -2.081668171172161734E-17, -4.930380657631307143E-31, 1.000000000000000000 ) ) ;
#9818 = EDGE_LOOP ( 'NONE', ( #5372, #8602, #11597, #3323 ) ) ;
#9819 = CYLINDRICAL_SURFACE ( 'NONE', #1144, 7.500000000000012434 ) ;
#9820 = CARTESIAN_POINT ( 'NONE',  ( -1037.337636019038882, 116.9882293220588991, -124.6807709998043521 ) ) ;
#9821 = CARTESIAN_POINT ( 'NONE',  ( -120.0000000000000000, 139.9999999999999716, -126.4213562373086575 ) ) ;
#9822 = CARTESIAN_POINT ( 'NONE',  ( -375.0000000000000568, 82.00000000000093792, -94.68077099980381206 ) ) ;
#9823 = DIRECTION ( 'NONE',  ( -0.000000000000000000, 1.000000000000000000, 7.930164461608263644E-17 ) ) ;
#9824 = EDGE_LOOP ( 'NONE', ( #3057, #124 ) ) ;
#9825 = EDGE_CURVE ( 'NONE', #1640, #3716, #3473, .T. ) ;
#9826 = CARTESIAN_POINT ( 'NONE',  ( -384.1383856924539373, 74.17476869750447577, -143.0957938661287301 ) ) ;
#9827 = CARTESIAN_POINT ( 'NONE',  ( -1047.392513188124212, 70.23666496464454667, -154.2940595301285214 ) ) ;
#9828 = ORIENTED_EDGE ( 'NONE', *, *, #4033, .T. ) ;
#9829 = PRESENTATION_LAYER_ASSIGNMENT (  '', '', ( #4897 ) ) ;
#9830 = CARTESIAN_POINT ( 'NONE',  ( -373.7989999032910191, 94.92607833831473840, -150.8034571341187586 ) ) ;
#9831 = CARTESIAN_POINT ( 'NONE',  ( -67.50000000000000000, 152.0000000000000000, -126.4213562373090696 ) ) ;
#9832 = CARTESIAN_POINT ( 'NONE',  ( -372.9400467759962226, 63.90640018081566609, -116.0698391000898511 ) ) ;
#9833 = CARTESIAN_POINT ( 'NONE',  ( 3.123963502971610252E-13, -6.000000000000006217, -88.92135623730948168 ) ) ;
#9834 = CYLINDRICAL_SURFACE ( 'NONE', #8463, 7.500000000000007105 ) ;
#9835 = EDGE_LOOP ( 'NONE', ( #8683, #10776, #8489, #5730 ) ) ;
#9836 = CARTESIAN_POINT ( 'NONE',  ( -1062.493403002509012, 61.99900353997395541, -149.7857175106634315 ) ) ;
#9837 = TOROIDAL_SURFACE ( 'NONE', #4518, 4.000000000000045297, 1.000000000000000000 ) ;
#9838 = CIRCLE ( 'NONE', #7047, 7.500000000000007105 ) ;
#9839 = ORIENTED_EDGE ( 'NONE', *, *, #5979, .T. ) ;
#9840 = ORIENTED_EDGE ( 'NONE', *, *, #1645, .T. ) ;
#9841 = CARTESIAN_POINT ( 'NONE',  ( 1.387778780781445676E-14, 0.000000000000000000, 133.9213562373095101 ) ) ;
#9842 = CARTESIAN_POINT ( 'NONE',  ( 20.00056164720817264, 178.7050872343423578, -124.4636624667101472 ) ) ;
#9843 = EDGE_CURVE ( 'NONE', #4515, #10844, #9617, .T. ) ;
#9844 = CARTESIAN_POINT ( 'NONE',  ( -1048.438004920983758, 39.66697241395321782, -122.7172756069793138 ) ) ;
#9845 = ADVANCED_FACE ( 'NONE', ( #705, #4417 ), #4673, .T. ) ;
#9846 = EDGE_CURVE ( 'NONE', #9369, #6223, #3285, .T. ) ;
#9847 = EDGE_LOOP ( 'NONE', ( #6994, #9114, #9162, #8832, #9883 ) ) ;
#9848 = DIRECTION ( 'NONE',  ( -1.000000000000000000, 0.000000000000000000, 0.000000000000000000 ) ) ;
#9849 = AXIS2_PLACEMENT_3D ( 'NONE', #4079, #8534, #10502 ) ;
#9850 = CARTESIAN_POINT ( 'NONE',  ( 1.414009460465297036E-14, -9.213203435596451385, -126.4213562373094959 ) ) ;
#9851 = VERTEX_POINT ( 'NONE', #5453 ) ;
#9852 = ORIENTED_EDGE ( 'NONE', *, *, #8193, .T. ) ;
#9853 = ORIENTED_EDGE ( 'NONE', *, *, #1799, .F. ) ;
#9854 = EDGE_CURVE ( 'NONE', #5830, #12174, #5936, .T. ) ;
#9855 = DIRECTION ( 'NONE',  ( 0.000000000000000000, -0.000000000000000000, -1.000000000000000000 ) ) ;
#9856 = VECTOR ( 'NONE', #4583, 1000.000000000000000 ) ;
#9857 = CLOSED_SHELL ( 'NONE', ( #6987, #8996, #9715, #7815, #1048, #3289, #6596, #10881, #10071, #6667 ) ) ;
#9858 = DIRECTION ( 'NONE',  ( 0.000000000000000000, 0.000000000000000000, 1.000000000000000000 ) ) ;
#9859 = DIRECTION ( 'NONE',  ( 0.000000000000000000, 0.000000000000000000, 1.000000000000000000 ) ) ;
#9860 = CARTESIAN_POINT ( 'NONE',  ( -952.1456544189251190, 108.1568929870907141, -99.57582448894486049 ) ) ;
#9861 = FACE_OUTER_BOUND ( 'NONE', #7923, .T. ) ;
#9862 = B_SPLINE_CURVE_WITH_KNOTS ( 'NONE', 3,
 ( #8959, #489, #10875, #4278, #8047, #11816 ),
 .UNSPECIFIED., .F., .F.,
 ( 4, 2, 4 ),
 ( 0.009719890944573138583, 0.01235036185894304236, 0.01498083277331294615 ),
 .UNSPECIFIED. ) ;
#9863 = VERTEX_POINT ( 'NONE', #3472 ) ;
#9864 = DIRECTION ( 'NONE',  ( -8.163404592832030268E-17, 1.000000000000000000, -0.000000000000000000 ) ) ;
#9865 = CARTESIAN_POINT ( 'NONE',  ( -3.161662739628749519E-15, 267.2792206135785591, -126.4213562373094959 ) ) ;
#9866 = ORIENTED_EDGE ( 'NONE', *, *, #5063, .T. ) ;
#9867 = DIRECTION ( 'NONE',  ( -1.000000000000000000, 0.000000000000000000, 0.000000000000000000 ) ) ;
#9868 = ADVANCED_FACE ( 'NONE', ( #8322 ), #6389, .F. ) ;
#9869 = ORIENTED_EDGE ( 'NONE', *, *, #10556, .F. ) ;
#9870 = CARTESIAN_POINT ( 'NONE',  ( -44.00000000000000000, 25.00000000000002132, -126.4213562373094959 ) ) ;
#9871 = CARTESIAN_POINT ( 'NONE',  ( -1037.773541645229670, 93.34895244571353601, -96.78565065507908116 ) ) ;
#9872 = CARTESIAN_POINT ( 'NONE',  ( -370.4401466759219375, 106.8513018378076822, -134.3428354745942102 ) ) ;
#9873 = CARTESIAN_POINT ( 'NONE',  ( -1065.000000000006594, 112.0000000000007105, -124.6807709998041531 ) ) ;
#9874 = CARTESIAN_POINT ( 'NONE',  ( -87.04832655144203102, 12.00000000000000000, -217.9289243767376831 ) ) ;
#9875 = EDGE_CURVE ( 'NONE', #8333, #8717, #6256, .T. ) ;
#9876 = FACE_OUTER_BOUND ( 'NONE', #1309, .T. ) ;
#9877 = CARTESIAN_POINT ( 'NONE',  ( -818.9962482452900758, 77.37998253221826417, -144.1405054422206717 ) ) ;
#9878 = CARTESIAN_POINT ( 'NONE',  ( -828.7892213480602095, 79.32116703283860204, -104.8603099499564877 ) ) ;
#9879 = CARTESIAN_POINT ( 'NONE',  ( -1065.000000000003865, 52.00000000000021316, -124.6807709998039826 ) ) ;
#9880 = CARTESIAN_POINT ( 'NONE',  ( -379.8598815838158202, 100.8093737612647658, -117.8752137794534320 ) ) ;
#9881 = ADVANCED_FACE ( 'NONE', ( #2613 ), #840, .F. ) ;
#9882 = CARTESIAN_POINT ( 'NONE',  ( -820.5220565119172988, 82.43903826675141033, -95.06393426016371961 ) ) ;
#9883 = ORIENTED_EDGE ( 'NONE', *, *, #7463, .T. ) ;
#9884 = CARTESIAN_POINT ( 'NONE',  ( -126.4213562373094959, -6.000000000000000000, 7.500000000000035527 ) ) ;
#9885 = CARTESIAN_POINT ( 'NONE',  ( -1013.875822516558969, 120.2710389253236940, -126.6442663926291061 ) ) ;
#9886 = CARTESIAN_POINT ( 'NONE',  ( 2.187692937179487324E-12, 163.9999999999999716, 76.07864376269050410 ) ) ;
#9887 = CARTESIAN_POINT ( 'NONE',  ( -126.4213562373094959, -6.000000000000000000, 2.255140518769849223E-14 ) ) ;
#9888 = B_SPLINE_CURVE_WITH_KNOTS ( 'NONE', 3,
 ( #7010, #3135, #10798, #4130, #8929, #4074, #1348, #222, #3079, #10855, #460, #4256, #9928, #5980, #8024, #4185, #7905, #11553 ),
 .UNSPECIFIED., .F., .F.,
 ( 4, 2, 2, 2, 2, 2, 2, 2, 4 ),
 ( 0.002543027922241140014, 0.003172111293043450644, 0.003801194663845760841, 0.004430278034648071038, 0.005059361405450381668, 0.005688444776252692299, 0.006317528147055002929, 0.006946611517857312693, 0.007575694888659623323 ),
 .UNSPECIFIED. ) ;
#9889 = DIRECTION ( 'NONE',  ( 0.000000000000000000, 1.000000000000000000, 0.000000000000000000 ) ) ;
#9890 = ORIENTED_EDGE ( 'NONE', *, *, #8108, .T. ) ;
#9891 = CARTESIAN_POINT ( 'NONE',  ( -1054.380968608931425, 114.0683136310379524, -124.6807709998043663 ) ) ;
#9892 = CARTESIAN_POINT ( 'NONE',  ( -382.3432055905735183, 68.36282604260088647, -139.3218746688176282 ) ) ;
#9893 = DIRECTION ( 'NONE',  ( 0.000000000000000000, -1.757987137413040192E-14, 1.000000000000000000 ) ) ;
#9894 = DIRECTION ( 'NONE',  ( -1.000000000000000000, 0.000000000000000000, 0.000000000000000000 ) ) ;
#9895 = CARTESIAN_POINT ( 'NONE',  ( -819.4917226271898016, 76.16439187810770761, -94.68015410868913762 ) ) ;
#9896 = DIRECTION ( 'NONE',  ( -0.000000000000000000, -1.000000000000000000, -0.000000000000000000 ) ) ;
#9897 = ORIENTED_EDGE ( 'NONE', *, *, #5776, .F. ) ;
#9898 = CARTESIAN_POINT ( 'NONE',  ( -954.2862664537763067, 55.36536439393486830, -141.4553492942758908 ) ) ;
#9899 = VECTOR ( 'NONE', #8392, 999.9999999999998863 ) ;
#9900 = ORIENTED_EDGE ( 'NONE', *, *, #7359, .T. ) ;
#9901 = DIRECTION ( 'NONE',  ( 0.000000000000000000, 0.000000000000000000, 1.000000000000000000 ) ) ;
#9902 = AXIS2_PLACEMENT_3D ( 'NONE', #7461, #6532, #5542 ) ;
#9903 = CARTESIAN_POINT ( 'NONE',  ( -1065.000000000006594, 52.38665522077229042, -118.7903414690683945 ) ) ;
#9904 = ORIENTED_EDGE ( 'NONE', *, *, #3877, .F. ) ;
#9905 = CARTESIAN_POINT ( 'NONE',  ( -150.0000000000000000, -9.213203435596451385, -126.4213562373084301 ) ) ;
#9906 = ORIENTED_EDGE ( 'NONE', *, *, #10601, .T. ) ;
#9907 = ORIENTED_EDGE ( 'NONE', *, *, #2893, .F. ) ;
#9908 = AXIS2_PLACEMENT_3D ( 'NONE', #10812, #2402, #7978 ) ;
#9909 = CARTESIAN_POINT ( 'NONE',  ( -1025.976186494711783, 52.68972726728017619, -126.6442663926293193 ) ) ;
#9910 = EDGE_CURVE ( 'NONE', #8054, #4859, #7114, .T. ) ;
#9911 = DIRECTION ( 'NONE',  ( 0.000000000000000000, 0.000000000000000000, -1.000000000000000000 ) ) ;
#9912 = CARTESIAN_POINT ( 'NONE',  ( 35.00000000000000000, 12.00000000000000000, 40.70327710424895429 ) ) ;
#9913 = ADVANCED_FACE ( 'NONE', ( #5524 ), #12153, .F. ) ;
#9914 = CARTESIAN_POINT ( 'NONE',  ( -60.00000000000000000, 152.0000000000000000, -126.4213562373090696 ) ) ;
#9915 = CARTESIAN_POINT ( 'NONE',  ( -1046.909978542194949, 84.99913997988220160, -95.06748246948046699 ) ) ;
#9916 = CARTESIAN_POINT ( 'NONE',  ( -305.0000000000000568, 24.00000000000000711, -89.68077099980384048 ) ) ;
#9917 = CIRCLE ( 'NONE', #8545, 1.000000000000000888 ) ;
#9918 = ORIENTED_EDGE ( 'NONE', *, *, #3822, .T. ) ;
#9919 = CARTESIAN_POINT ( 'NONE',  ( -372.8632101103306695, 63.61025241748026815, -116.7299017350923833 ) ) ;
#9920 = ORIENTED_EDGE ( 'NONE', *, *, #4202, .F. ) ;
#9921 = DIRECTION ( 'NONE',  ( 0.000000000000000000, 0.000000000000000000, 1.000000000000000000 ) ) ;
#9922 = EDGE_LOOP ( 'NONE', ( #10093, #6946 ) ) ;
#9923 = DIRECTION ( 'NONE',  ( -8.163404592832030268E-17, 1.000000000000000000, -0.000000000000000000 ) ) ;
#9924 = CARTESIAN_POINT ( 'NONE',  ( -795.0000000000004547, 76.10956187831470743, -95.06748246948018277 ) ) ;
#9925 = LINE ( 'NONE', #2443, #4895 ) ;
#9926 = CARTESIAN_POINT ( 'NONE',  ( -21.06782942783708634, 181.2569958439586912, -125.9973154456346407 ) ) ;
#9927 = CARTESIAN_POINT ( 'NONE',  ( 21.06230101187101056, 180.1909031182395893, -126.4302698477766995 ) ) ;
#9928 = CARTESIAN_POINT ( 'NONE',  ( 19.87222927861654043, 180.0711623112485711, -122.4236614295827081 ) ) ;
#9929 = EDGE_CURVE ( 'NONE', #11819, #9863, #11955, .T. ) ;
#9930 = DIRECTION ( 'NONE',  ( 1.000000000000000000, 0.000000000000000000, -0.000000000000000000 ) ) ;
#9931 = AXIS2_PLACEMENT_3D ( 'NONE', #473, #10808, #4268 ) ;
#9932 = EDGE_CURVE ( 'NONE', #8245, #5183, #5851, .T. ) ;
#9933 = FACE_BOUND ( 'NONE', #3876, .T. ) ;
#9934 = CARTESIAN_POINT ( 'NONE',  ( -379.2306375576939672, 62.11345676130450499, -122.4830476075849788 ) ) ;
#9935 = PRODUCT_DEFINITION ( 'UNKNOWN', '', #3670, #11477 ) ;
#9936 = CARTESIAN_POINT ( 'NONE',  ( -822.2117862628927014, 83.41691093530795342, -95.20655667354223795 ) ) ;
#9937 = EDGE_LOOP ( 'NONE', ( #7065, #2464, #3218, #5513 ) ) ;
#9938 = DIRECTION ( 'NONE',  ( 0.000000000000000000, 0.000000000000000000, -1.000000000000000000 ) ) ;
#9939 = CARTESIAN_POINT ( 'NONE',  ( -1060.756016675586807, 112.8516620848305934, -124.6807709998040821 ) ) ;
#9940 = DIRECTION ( 'NONE',  ( 0.000000000000000000, 1.000000000000000000, -0.000000000000000000 ) ) ;
#9941 = DIRECTION ( 'NONE',  ( -1.000000000000000000, -0.000000000000000000, -0.000000000000000000 ) ) ;
#9942 = DIRECTION ( 'NONE',  ( 0.000000000000000000, 0.000000000000000000, 1.000000000000000000 ) ) ;
#9943 = AXIS2_PLACEMENT_3D ( 'NONE', #4674, #5706, #10404 ) ;
#9944 = VECTOR ( 'NONE', #3453, 1000.000000000000000 ) ;
#9945 = DIRECTION ( 'NONE',  ( -1.000000000000000000, 0.000000000000000000, 0.000000000000000000 ) ) ;
#9946 = EDGE_LOOP ( 'NONE', ( #6260, #1845, #6602, #1004 ) ) ;
#9947 = EDGE_CURVE ( 'NONE', #5383, #125, #12187, .T. ) ;
#9948 = ORIENTED_EDGE ( 'NONE', *, *, #4342, .T. ) ;
#9949 = FACE_OUTER_BOUND ( 'NONE', #11614, .T. ) ;
#9950 = CARTESIAN_POINT ( 'NONE',  ( -819.8389179520123662, 63.91331975908080665, -154.2940595301278677 ) ) ;
#9951 = CARTESIAN_POINT ( 'NONE',  ( 45.53315400109643463, 12.00000000000000000, -245.3419396193597493 ) ) ;
#9952 = AXIS2_PLACEMENT_3D ( 'NONE', #5940, #3157, #1073 ) ;
#9953 = CIRCLE ( 'NONE', #3842, 20.00000000000000000 ) ;
#9954 = DIRECTION ( 'NONE',  ( 0.000000000000000000, 0.000000000000000000, 1.000000000000000000 ) ) ;
#9955 = CARTESIAN_POINT ( 'NONE',  ( 35.00000000000000000, 152.0000000000000000, -89.68077099980384048 ) ) ;
#9956 = CIRCLE ( 'NONE', #5407, 7.500000000000007105 ) ;
#9957 = CARTESIAN_POINT ( 'NONE',  ( 1.734723475976807094E-15, 180.2041921146324910, -179.7948474705909234 ) ) ;
#9958 = CARTESIAN_POINT ( 'NONE',  ( -371.8264734514620500, 61.12950623280156037, -106.3821846224840755 ) ) ;
#9959 = CARTESIAN_POINT ( 'NONE',  ( -822.0694275022420925, 73.99112643935335143, -94.71034476858436335 ) ) ;
#9960 = EDGE_LOOP ( 'NONE', ( #6693, #5611, #6564, #3239 ) ) ;
#9961 = CARTESIAN_POINT ( 'NONE',  ( -853.8938961404190877, 37.86297855175782701, -146.0307792196449554 ) ) ;
#9962 = ORIENTED_EDGE ( 'NONE', *, *, #10971, .F. ) ;
#9963 = VECTOR ( 'NONE', #6088, 1000.000000000000000 ) ;
#9964 = LINE ( 'NONE', #11767, #6049 ) ;
#9965 = CARTESIAN_POINT ( 'NONE',  ( -6.360897667028196044E-14, -494.9999999999998863, -141.4213562373094817 ) ) ;
#9966 = CARTESIAN_POINT ( 'NONE',  ( -20.75022707385176801, 180.8238523145130330, -123.4308975868758580 ) ) ;
#9967 = EDGE_LOOP ( 'NONE', ( #8372, #1225, #11691, #5572 ) ) ;
#9968 = CARTESIAN_POINT ( 'NONE',  ( 0.000000000000000000, -6.000000000000000000, -126.4213562373094959 ) ) ;
#9969 = FACE_OUTER_BOUND ( 'NONE', #11286, .T. ) ;
#9970 = ORIENTED_EDGE ( 'NONE', *, *, #3945, .F. ) ;
#9971 = FACE_OUTER_BOUND ( 'NONE', #6996, .T. ) ;
#9972 = AXIS2_PLACEMENT_3D ( 'NONE', #4294, #1565, #10221 ) ;
#9973 = CIRCLE ( 'NONE', #3449, 4.000000000000003553 ) ;
#9974 = LINE ( 'NONE', #9163, #3086 ) ;
#9975 = EDGE_LOOP ( 'NONE', ( #8329, #452, #2229, #9531 ) ) ;
#9976 = CARTESIAN_POINT ( 'NONE',  ( 126.4213562373094959, 12.00000000000000000, 7.500000000000007105 ) ) ;
#9977 = DIRECTION ( 'NONE',  ( -1.000000000000000000, 0.000000000000000000, 0.000000000000000000 ) ) ;
#9978 =( GEOMETRIC_REPRESENTATION_CONTEXT ( 3 ) GLOBAL_UNCERTAINTY_ASSIGNED_CONTEXT ( ( #212 ) ) GLOBAL_UNIT_ASSIGNED_CONTEXT ( ( #7205, #11898, #8716 ) ) REPRESENTATION_CONTEXT ( 'NONE', 'WORKASPACE' ) );
#9979 = CARTESIAN_POINT ( 'NONE',  ( -1056.430032577878137, 71.19035303699463668, -95.06748246948046699 ) ) ;
#9980 = CARTESIAN_POINT ( 'NONE',  ( 8.500000000000007105, 167.0000000000000000, -124.6807709998038405 ) ) ;
#9981 = EDGE_CURVE ( 'NONE', #8885, #2093, #9362, .T. ) ;
#9982 = ORIENTED_EDGE ( 'NONE', *, *, #10704, .T. ) ;
#9983 = CARTESIAN_POINT ( 'NONE',  ( 9.371890508914830252E-13, -6.000000000000005329, -36.42135623730949590 ) ) ;
#9984 = VERTEX_POINT ( 'NONE', #12210 ) ;
#9985 = FACE_OUTER_BOUND ( 'NONE', #9152, .T. ) ;
#9986 = CARTESIAN_POINT ( 'NONE',  ( -35.00000000000000000, 164.0000000000000000, -124.6807709998038689 ) ) ;
#9987 = ORIENTED_EDGE ( 'NONE', *, *, #8965, .F. ) ;
#9988 = CARTESIAN_POINT ( 'NONE',  ( -6.360897667028196044E-14, -492.9999999999998863, -141.4213562373094817 ) ) ;
#9989 = CARTESIAN_POINT ( 'NONE',  ( -1047.626240907246483, 63.12837257276869707, -96.78565065507969223 ) ) ;
#9990 = CARTESIAN_POINT ( 'NONE',  ( -6.165341064827238593E-15, 8.014718854569425233, 4.118099735505519554 ) ) ;
#9991 = PRODUCT_DEFINITION_FORMATION_WITH_SPECIFIED_SOURCE ( 'ANY', '', #10588, .NOT_KNOWN. ) ;
#9992 = CARTESIAN_POINT ( 'NONE',  ( -21.06346387521529806, 180.5375120120260135, -126.3982203091088508 ) ) ;
#9993 = CIRCLE ( 'NONE', #4679, 1.500000000000000666 ) ;
#9994 = CARTESIAN_POINT ( 'NONE',  ( -1024.722591077092829, 118.3980260646366958, -118.7903414690678403 ) ) ;
#9995 = LINE ( 'NONE', #10739, #5301 ) ;
#9996 = CARTESIAN_POINT ( 'NONE',  ( -820.5015944640188081, 74.92794535927947663, -143.3902763353420369 ) ) ;
#9997 = DIRECTION ( 'NONE',  ( 0.000000000000000000, -0.000000000000000000, 1.000000000000000000 ) ) ;
#9998 = CARTESIAN_POINT ( 'NONE',  ( -144.0488662551579182, 0.000000000000000000, -139.4077238332691877 ) ) ;
#9999 = EDGE_CURVE ( 'NONE', #6258, #6415, #1324, .T. ) ;
#10000 = AXIS2_PLACEMENT_3D ( 'NONE', #652, #9923, #10850 ) ;
#10001 = EDGE_LOOP ( 'NONE', ( #6624, #5157, #1505, #11857 ) ) ;
#10002 = CARTESIAN_POINT ( 'NONE',  ( -1013.875822516560447, 120.2710389253235519, -122.7172756069789017 ) ) ;
#10003 = LINE ( 'NONE', #5418, #6354 ) ;
#10004 = LINE ( 'NONE', #7225, #11013 ) ;
#10005 = FACE_OUTER_BOUND ( 'NONE', #7256, .T. ) ;
#10006 = EDGE_CURVE ( 'NONE', #8885, #9472, #9001, .T. ) ;
#10007 = FACE_OUTER_BOUND ( 'NONE', #4318, .T. ) ;
#10008 = ORIENTED_EDGE ( 'NONE', *, *, #654, .F. ) ;
#10009 = VECTOR ( 'NONE', #8839, 1000.000000000000000 ) ;
#10010 = ORIENTED_EDGE ( 'NONE', *, *, #2696, .F. ) ;
#10011 = CARTESIAN_POINT ( 'NONE',  ( 19.87720992741833825, 179.7310258856144287, -122.4675742865357932 ) ) ;
#10012 = CARTESIAN_POINT ( 'NONE',  ( -19.83216922734808207, 179.9533482554023180, -127.2663209614022293 ) ) ;
#10013 = DIRECTION ( 'NONE',  ( 1.186840563529527301E-16, -1.000000000000000000, 0.000000000000000000 ) ) ;
#10014 = CARTESIAN_POINT ( 'NONE',  ( -955.9230626098308221, 78.80814421416198456, -154.2940595301282372 ) ) ;
#10015 = CARTESIAN_POINT ( 'NONE',  ( 0.8038475772933637575, -10.39230484541326405, -2.038422702671202938E-16 ) ) ;
#10016 = CARTESIAN_POINT ( 'NONE',  ( 35.00000000000000000, 12.00000000000002309, -159.6807709998040252 ) ) ;
#10017 = DIRECTION ( 'NONE',  ( -8.163404592832030268E-17, 1.000000000000000000, -0.000000000000000000 ) ) ;
#10018 = CARTESIAN_POINT ( 'NONE',  ( -826.8800118742810810, 74.69996070206661898, -94.68424396577464108 ) ) ;
#10019 = AXIS2_PLACEMENT_3D ( 'NONE', #2551, #636, #8122 ) ;
#10020 = EDGE_CURVE ( 'NONE', #10076, #6923, #11591, .T. ) ;
#10021 = EDGE_LOOP ( 'NONE', ( #8479, #2661, #7477, #8670 ) ) ;
#10022 = CARTESIAN_POINT ( 'NONE',  ( -1062.810894920117335, 52.92335929224806534, -141.4553492942755781 ) ) ;
#10023 = VERTEX_POINT ( 'NONE', #2624 ) ;
#10024 = ADVANCED_FACE ( 'NONE', ( #1709 ), #4743, .F. ) ;
#10025 = EDGE_CURVE ( 'NONE', #6648, #6415, #8568, .T. ) ;
#10026 = ORIENTED_EDGE ( 'NONE', *, *, #3212, .T. ) ;
#10027 = VECTOR ( 'NONE', #6541, 1000.000000000000000 ) ;
#10028 = CARTESIAN_POINT ( 'NONE',  ( -21.06507840625382499, 180.7491199079335047, -126.3364105811339329 ) ) ;
#10029 = ORIENTED_EDGE ( 'NONE', *, *, #11739, .T. ) ;
#10030 = CARTESIAN_POINT ( 'NONE',  ( -370.0960371382928429, 56.26061672099882571, -130.5900565961996449 ) ) ;
#10031 = CARTESIAN_POINT ( 'NONE',  ( 1.387778780781445676E-14, 0.000000000000000000, 133.9213562373095101 ) ) ;
#10032 = ORIENTED_EDGE ( 'NONE', *, *, #8881, .F. ) ;
#10033 = ADVANCED_FACE ( 'NONE', ( #5468 ), #3541, .T. ) ;
#10034 = CIRCLE ( 'NONE', #4717, 7.500000000000020428 ) ;
#10035 = DIRECTION ( 'NONE',  ( 1.000000000000000000, 0.000000000000000000, 0.000000000000000000 ) ) ;
#10036 = ORIENTED_EDGE ( 'NONE', *, *, #11359, .F. ) ;
#10037 = CARTESIAN_POINT ( 'NONE',  ( -954.5692209181572707, 49.02792041507773746, -126.6442663926294045 ) ) ;
#10038 = AXIS2_PLACEMENT_3D ( 'NONE', #5370, #12061, #7364 ) ;
#10039 = CYLINDRICAL_SURFACE ( 'NONE', #10953, 7.500000000000007105 ) ;
#10040 = CARTESIAN_POINT ( 'NONE',  ( 30.00000000000000000, -492.9999999999998863, -30.00000000000000000 ) ) ;
#10041 = AXIS2_PLACEMENT_3D ( 'NONE', #8845, #5010, #311 ) ;
#10042 = CARTESIAN_POINT ( 'NONE',  ( -1012.226803665789134, 93.06815595962675047, -95.06748246948018277 ) ) ;
#10043 = CARTESIAN_POINT ( 'NONE',  ( -154.5043356068770493, 12.00000000000000000, -102.0666613060160302 ) ) ;
#10044 = DIRECTION ( 'NONE',  ( -1.000000000000000000, -3.061276722312011504E-17, -0.000000000000000000 ) ) ;
#10045 = EDGE_LOOP ( 'NONE', ( #10142, #7647, #10934, #5278 ) ) ;
#10046 = CARTESIAN_POINT ( 'NONE',  ( 56.53599999999998715, 0.000000000000000000, 5.999999999999999112 ) ) ;
#10047 = FACE_OUTER_BOUND ( 'NONE', #7249, .T. ) ;
#10048 = ORIENTED_EDGE ( 'NONE', *, *, #1390, .F. ) ;
#10049 = CARTESIAN_POINT ( 'NONE',  ( -822.5362431349451526, 83.50721794775202511, -154.1394416282527970 ) ) ;
#10050 = CARTESIAN_POINT ( 'NONE',  ( -1031.794838716553841, 81.34535957697958963, -94.48732055948609343 ) ) ;
#10051 = CARTESIAN_POINT ( 'NONE',  ( 0.01899995639453432028, 8.236198097127171991, 3.734486434573631719 ) ) ;
#10052 = CARTESIAN_POINT ( 'NONE',  ( -1065.000000000003865, 112.0000000000008527, -126.6442663926290493 ) ) ;
#10053 = LINE ( 'NONE', #9121, #2173 ) ;
#10054 = DIRECTION ( 'NONE',  ( 1.000000000000000000, 0.000000000000000000, 0.000000000000000000 ) ) ;
#10055 = CARTESIAN_POINT ( 'NONE',  ( 35.00000000000000000, 81.99999999999998579, 260.3192290001960032 ) ) ;
#10056 = DIRECTION ( 'NONE',  ( 0.000000000000000000, 0.000000000000000000, 1.000000000000000000 ) ) ;
#10057 = VECTOR ( 'NONE', #4498, 1000.000000000000000 ) ;
#10058 = CARTESIAN_POINT ( 'NONE',  ( 126.4213562373094959, 12.00000000000000000, -6.938893903907228378E-15 ) ) ;
#10059 = EDGE_LOOP ( 'NONE', ( #6133, #9852, #2415, #5485, #10514, #7105 ) ) ;
#10060 = LINE ( 'NONE', #667, #1130 ) ;
#10061 = CARTESIAN_POINT ( 'NONE',  ( -951.4198147059590838, 125.0824040815807194, -122.7172756069790864 ) ) ;
#10062 = CARTESIAN_POINT ( 'NONE',  ( -795.0000000000043201, 82.00000000000039790, -124.6807709998041105 ) ) ;
#10063 = DIRECTION ( 'NONE',  ( -8.163404592832030268E-17, 1.000000000000000000, -0.000000000000000000 ) ) ;
#10064 = EDGE_CURVE ( 'NONE', #2669, #8433, #5536, .T. ) ;
#10065 = CARTESIAN_POINT ( 'NONE',  ( 19.94309760505412399, 182.0081148946152041, -123.1517843831254169 ) ) ;
#10066 = EDGE_CURVE ( 'NONE', #647, #4463, #6847, .T. ) ;
#10067 = ORIENTED_EDGE ( 'NONE', *, *, #6839, .F. ) ;
#10068 = DIRECTION ( 'NONE',  ( 1.000000000000000000, 0.000000000000000000, 0.000000000000000000 ) ) ;
#10069 = CARTESIAN_POINT ( 'NONE',  ( -384.9422428523002964, 79.88598318847526514, -144.5779090198339532 ) ) ;
#10070 = CARTESIAN_POINT ( 'NONE',  ( -955.0423082396526979, 101.0797422464698769, -152.5758913445288272 ) ) ;
#10071 = ADVANCED_FACE ( 'NONE', ( #436 ), #6009, .T. ) ;
#10072 = DIRECTION ( 'NONE',  ( 0.000000000000000000, 0.000000000000000000, 1.000000000000000000 ) ) ;
#10073 = FACE_OUTER_BOUND ( 'NONE', #2919, .T. ) ;
#10074 = CARTESIAN_POINT ( 'NONE',  ( -955.3297122972861644, 93.84065249268903131, -154.2940595301280950 ) ) ;
#10075 = CARTESIAN_POINT ( 'NONE',  ( -823.8285638327238303, 78.67432280806536937, -89.68077099980398259 ) ) ;
#10076 = VERTEX_POINT ( 'NONE', #1112 ) ;
#10077 = CARTESIAN_POINT ( 'NONE',  ( -240.0000000000000000, -9.213203435596478030, -126.4213562373078190 ) ) ;
#10078 =( NAMED_UNIT ( * ) PLANE_ANGLE_UNIT ( ) SI_UNIT ( $, .RADIAN. ) );
#10079 = ORIENTED_EDGE ( 'NONE', *, *, #7525, .T. ) ;
#10080 = DIRECTION ( 'NONE',  ( -0.000000000000000000, -1.000000000000000000, -0.000000000000000000 ) ) ;
#10081 = CARTESIAN_POINT ( 'NONE',  ( -1028.007066121607295, 60.50166182213178701, -146.0307792196450123 ) ) ;
#10082 =( REPRESENTATION_RELATIONSHIP ('NONE','NONE', #12149, #1102 ) REPRESENTATION_RELATIONSHIP_WITH_TRANSFORMATION ( #664 )SHAPE_REPRESENTATION_RELATIONSHIP( ) );
#10083 = VERTEX_POINT ( 'NONE', #3518 ) ;
#10084 = VECTOR ( 'NONE', #6212, 1000.000000000000000 ) ;
#10085 = ORIENTED_EDGE ( 'NONE', *, *, #2424, .F. ) ;
#10086 = EDGE_CURVE ( 'NONE', #2780, #6278, #5665, .T. ) ;
#10087 = CARTESIAN_POINT ( 'NONE',  ( -21.06429661575627676, 179.7721861010548139, -126.3654905360901068 ) ) ;
#10088 = EDGE_LOOP ( 'NONE', ( #5062, #7933 ) ) ;
#10089 = CARTESIAN_POINT ( 'NONE',  ( -370.0632692633016063, 56.17797598930829395, -130.0988530496388478 ) ) ;
#10090 = DIRECTION ( 'NONE',  ( -1.000000000000000000, -1.156482317317870492E-16, 0.000000000000000000 ) ) ;
#10091 = ORIENTED_EDGE ( 'NONE', *, *, #6698, .T. ) ;
#10092 = CIRCLE ( 'NONE', #835, 5.000000000000115463 ) ;
#10093 = ORIENTED_EDGE ( 'NONE', *, *, #7667, .T. ) ;
#10094 = CARTESIAN_POINT ( 'NONE',  ( -1062.996098538724254, 47.98024286075312261, -130.5712005305402101 ) ) ;
#10095 = DIRECTION ( 'NONE',  ( 0.000000000000000000, 0.000000000000000000, 1.000000000000000000 ) ) ;
#10096 = AXIS2_PLACEMENT_3D ( 'NONE', #1243, #411, #7856 ) ;
#10097 = DIRECTION ( 'NONE',  ( -0.000000000000000000, 1.000000000000000000, -0.000000000000000000 ) ) ;
#10098 = EDGE_CURVE ( 'NONE', #7181, #11998, #8820, .T. ) ;
#10099 = CARTESIAN_POINT ( 'NONE',  ( -955.6263874535618470, 86.32439835342511003, -94.48732055948597974 ) ) ;
#10100 = DIRECTION ( 'NONE',  ( 0.000000000000000000, 1.000000000000000000, 0.000000000000000000 ) ) ;
#10101 = FACE_BOUND ( 'NONE', #5217, .T. ) ;
#10102 = AXIS2_PLACEMENT_3D ( 'NONE', #2287, #6180, #9945 ) ;
#10103 = EDGE_LOOP ( 'NONE', ( #9465, #6477, #6070, #8555 ) ) ;
#10104 = DIRECTION ( 'NONE',  ( -0.1214029594221266301, -0.3196865710829014384, -0.9397136892228434846 ) ) ;
#10105 = DIRECTION ( 'NONE',  ( 1.000000000000000000, 0.000000000000000000, 0.000000000000000000 ) ) ;
#10106 = DIRECTION ( 'NONE',  ( -8.163404592832031500E-17, 1.000000000000000000, 0.000000000000000000 ) ) ;
#10107 = ORIENTED_EDGE ( 'NONE', *, *, #10649, .F. ) ;
#10108 = CARTESIAN_POINT ( 'NONE',  ( -820.7809001343154023, 82.65155347377678652, -154.2690219959281421 ) ) ;
#10109 = CARTESIAN_POINT ( 'NONE',  ( -995.4135022096149896, 71.70161378084165449, -95.06748246948046699 ) ) ;
#10110 = CARTESIAN_POINT ( 'NONE',  ( 3.133148353965215262E-13, -6.000000000000004441, -103.9213562373094959 ) ) ;
#10111 = PLANE ( 'NONE',  #3888 ) ;
#10112 = CARTESIAN_POINT ( 'NONE',  ( 1.479627290717497352E-14, 0.000000000000000000, 118.9213562373094817 ) ) ;
#10113 = DIRECTION ( 'NONE',  ( -1.000000000000000000, 0.000000000000000000, 0.000000000000000000 ) ) ;
#10114 = AXIS2_PLACEMENT_3D ( 'NONE', #4802, #1964, #2199 ) ;
#10115 = CARTESIAN_POINT ( 'NONE',  ( -827.1569714199375767, 74.92915896788937857, -105.9707980921569117 ) ) ;
#10116 = CARTESIAN_POINT ( 'NONE',  ( -20.86426071607942845, 178.9745188154266771, -123.9720018873370009 ) ) ;
#10117 = DIRECTION ( 'NONE',  ( 0.000000000000000000, 1.000000000000000000, 0.000000000000000000 ) ) ;
#10118 = VERTEX_POINT ( 'NONE', #2537 ) ;
#10119 = CARTESIAN_POINT ( 'NONE',  ( -370.0557944711135292, 56.15912500487524994, -119.3740868421776327 ) ) ;
#10120 = ORIENTED_EDGE ( 'NONE', *, *, #4672, .T. ) ;
#10121 = DIRECTION ( 'NONE',  ( -1.000000000000000000, -3.061276722312011504E-17, 0.000000000000000000 ) ) ;
#10122 = CARTESIAN_POINT ( 'NONE',  ( -1045.864486809339951, 115.5688325305733741, -122.7172756069790438 ) ) ;
#10123 = CARTESIAN_POINT ( 'NONE',  ( -1065.000000000003865, 52.00000000000021316, -124.6807709998039826 ) ) ;
#10124 = FACE_OUTER_BOUND ( 'NONE', #7821, .T. ) ;
#10125 = DIRECTION ( 'NONE',  ( 1.000000000000000000, 0.000000000000000000, 0.000000000000000000 ) ) ;
#10126 = CARTESIAN_POINT ( 'NONE',  ( 19.98725040941994635, 181.3779265047164415, -125.6147582845246973 ) ) ;
#10127 = ORIENTED_EDGE ( 'NONE', *, *, #7473, .T. ) ;
#10128 = VECTOR ( 'NONE', #7248, 1000.000000000000000 ) ;
#10129 = EDGE_LOOP ( 'NONE', ( #11525, #4340, #8174, #1559 ) ) ;
#10130 = CARTESIAN_POINT ( 'NONE',  ( -277.5000000000000000, -9.213203435596478030, -126.4213562373076059 ) ) ;
#10131 = DIRECTION ( 'NONE',  ( 0.000000000000000000, 1.000000000000000000, 0.000000000000000000 ) ) ;
#10132 = CARTESIAN_POINT ( 'NONE',  ( -1055.176328965298808, 98.13059730676609149, -149.7857175106632326 ) ) ;
#10133 = CARTESIAN_POINT ( 'NONE',  ( -379.1811916902539679, 101.9683303498903513, -125.9862397059319505 ) ) ;
#10134 = EDGE_CURVE ( 'NONE', #4463, #4959, #8527, .T. ) ;
#10135 = CARTESIAN_POINT ( 'NONE',  ( -270.0000000000000000, 24.00000000000000711, -126.4213562373076059 ) ) ;
#10136 = DIRECTION ( 'NONE',  ( 0.000000000000000000, 0.000000000000000000, 1.000000000000000000 ) ) ;
#10137 = EDGE_LOOP ( 'NONE', ( #8938, #9023 ) ) ;
#10138 = CARTESIAN_POINT ( 'NONE',  ( -45.53315400109751465, 12.00000000000000000, -237.8419396193594650 ) ) ;
#10139 = AXIS2_PLACEMENT_3D ( 'NONE', #12086, #2614, #1945 ) ;
#10140 =( NAMED_UNIT ( * ) SI_UNIT ( $, .STERADIAN. ) SOLID_ANGLE_UNIT ( ) );
#10141 = EDGE_CURVE ( 'NONE', #1000, #11268, #10434, .T. ) ;
#10142 = ORIENTED_EDGE ( 'NONE', *, *, #2299, .F. ) ;
#10143 = DIRECTION ( 'NONE',  ( 3.061276722312011504E-17, -1.000000000000000000, 0.000000000000000000 ) ) ;
#10144 = CARTESIAN_POINT ( 'NONE',  ( -1020.430183747032629, 74.13649791779326392, -152.5758913445297651 ) ) ;
#10145 = VERTEX_POINT ( 'NONE', #7310 ) ;
#10146 = ORIENTED_EDGE ( 'NONE', *, *, #2447, .T. ) ;
#10147 = TOROIDAL_SURFACE ( 'NONE', #9153, 19.00000000000000000, 1.000000000000000000 ) ;
#10148 = CIRCLE ( 'NONE', #5790, 7.500000000000007994 ) ;
#10149 = DIRECTION ( 'NONE',  ( 0.000000000000000000, 0.000000000000000000, 1.000000000000000000 ) ) ;
#10150 = VERTEX_POINT ( 'NONE', #3759 ) ;
#10151 = CARTESIAN_POINT ( 'NONE',  ( -380.0389975087255152, 63.50064549581343698, -132.3938157233661457 ) ) ;
#10152 = CARTESIAN_POINT ( 'NONE',  ( -119.9999999999999858, -9.213203435596451385, -126.4213562373086575 ) ) ;
#10153 = EDGE_CURVE ( 'NONE', #206, #1690, #2599, .T. ) ;
#10154 = ORIENTED_EDGE ( 'NONE', *, *, #1452, .F. ) ;
#10155 = ADVANCED_FACE ( 'NONE', ( #157 ), #6312, .T. ) ;
#10156 = ORIENTED_EDGE ( 'NONE', *, *, #5912, .T. ) ;
#10157 = CARTESIAN_POINT ( 'NONE',  ( -1028.581275045468146, 51.02622020309988216, -130.5712005305406080 ) ) ;
#10158 = AXIS2_PLACEMENT_3D ( 'NONE', #6081, #5960, #8746 ) ;
#10159 = CIRCLE ( 'NONE', #8778, 57.99999999999999289 ) ;
#10160 = DIRECTION ( 'NONE',  ( -0.000000000000000000, 1.000000000000000000, -0.000000000000000000 ) ) ;
#10161 = CARTESIAN_POINT ( 'NONE',  ( 0.000000000000000000, 10.39230484541327115, -2.602085213965207092E-15 ) ) ;
#10162 = CARTESIAN_POINT ( 'NONE',  ( 19.98390859781245510, 179.2016144824152093, -125.7887931655865685 ) ) ;
#10163 = CARTESIAN_POINT ( 'NONE',  ( -819.8389179520128209, 63.91331975908082086, -95.06748246948014014 ) ) ;
#10164 = CARTESIAN_POINT ( 'NONE',  ( 144.0488662551573782, 0.000000000000000000, -146.9077238332702109 ) ) ;
#10165 = DIRECTION ( 'NONE',  ( 0.000000000000000000, 1.000000000000000000, 0.000000000000000000 ) ) ;
#10166 = CARTESIAN_POINT ( 'NONE',  ( -795.0000000000047748, 52.00000000000024158, -122.7172756069790154 ) ) ;
#10167 = AXIS2_PLACEMENT_3D ( 'NONE', #3291, #9855, #9037 ) ;
#10168 = VERTEX_POINT ( 'NONE', #7242 ) ;
#10169 = CARTESIAN_POINT ( 'NONE',  ( -819.0830098007990046, 80.28235241365167951, -144.6091609974195080 ) ) ;
#10170 = CARTESIAN_POINT ( 'NONE',  ( 0.000000000000000000, 0.000000000000000000, 0.000000000000000000 ) ) ;
#10171 = FACE_OUTER_BOUND ( 'NONE', #12011, .T. ) ;
#10172 = DIRECTION ( 'NONE',  ( 0.000000000000000000, 0.000000000000000000, 1.000000000000000000 ) ) ;
#10173 = EDGE_LOOP ( 'NONE', ( #9354, #8412, #8044, #4966 ) ) ;
#10174 = ADVANCED_FACE ( 'NONE', ( #7592 ), #4810, .T. ) ;
#10175 = CARTESIAN_POINT ( 'NONE',  ( -1015.517346982276649, 86.95624952299064603, -94.48732055948629238 ) ) ;
#10176 = EDGE_CURVE ( 'NONE', #6019, #11124, #11008, .T. ) ;
#10177 = CARTESIAN_POINT ( 'NONE',  ( -35.00000000000000000, 12.00000000000002309, -159.6807709998040252 ) ) ;
#10178 = FACE_OUTER_BOUND ( 'NONE', #8227, .T. ) ;
#10179 =( GEOMETRIC_REPRESENTATION_CONTEXT ( 3 ) GLOBAL_UNCERTAINTY_ASSIGNED_CONTEXT ( ( #1387 ) ) GLOBAL_UNIT_ASSIGNED_CONTEXT ( ( #8332, #6525, #7573 ) ) REPRESENTATION_CONTEXT ( 'NONE', 'WORKASPACE' ) );
#10180 = CARTESIAN_POINT ( 'NONE',  ( -822.5144771496169369, 73.83866123373404378, -106.4215885538519615 ) ) ;
#10181 = CARTESIAN_POINT ( 'NONE',  ( -824.1558762432716776, 73.68222816774701300, -142.8690915370043228 ) ) ;
#10182 = EDGE_LOOP ( 'NONE', ( #8313, #11465, #7786, #9708 ) ) ;
#10183 = ORIENTED_EDGE ( 'NONE', *, *, #4290, .F. ) ;
#10184 = DIRECTION ( 'NONE',  ( -0.000000000000000000, 1.000000000000000000, 0.000000000000000000 ) ) ;
#10185 = CONTEXT_DEPENDENT_SHAPE_REPRESENTATION ( #5023, #10687 ) ;
#10186 = AXIS2_PLACEMENT_3D ( 'NONE', #9433, #6586, #4619 ) ;
#10187 = ORIENTED_EDGE ( 'NONE', *, *, #11837, .T. ) ;
#10188 = DIRECTION ( 'NONE',  ( -3.061276722312011504E-17, 1.000000000000000000, 0.000000000000000000 ) ) ;
#10189 = CARTESIAN_POINT ( 'NONE',  ( -951.4198147059589701, 125.0824040815807194, -124.6807709998040252 ) ) ;
#10190 = DIRECTION ( 'NONE',  ( -1.000000000000000000, 0.000000000000000000, 0.000000000000000000 ) ) ;
#10191 = CARTESIAN_POINT ( 'NONE',  ( 1.561981751485805177E-12, 0.000000000000000000, 23.57864376269050410 ) ) ;
#10192 = DIRECTION ( 'NONE',  ( 0.000000000000000000, 1.000000000000000000, 0.000000000000000000 ) ) ;
#10193 = CARTESIAN_POINT ( 'NONE',  ( 20.88840428458409448, 181.5134543962125804, -124.1041536322683783 ) ) ;
#10194 = ORIENTED_EDGE ( 'NONE', *, *, #10176, .F. ) ;
#10195 = ORIENTED_EDGE ( 'NONE', *, *, #5497, .T. ) ;
#10196 = AXIS2_PLACEMENT_3D ( 'NONE', #9038, #10784, #11661 ) ;
#10197 = FACE_OUTER_BOUND ( 'NONE', #7160, .T. ) ;
#10198 = LINE ( 'NONE', #7356, #1281 ) ;
#10199 = CARTESIAN_POINT ( 'NONE',  ( -903.4746773471192682, 104.0883302344920480, -152.5758913445288272 ) ) ;
#10200 = DIRECTION ( 'NONE',  ( -1.000000000000000000, 0.000000000000000000, 0.000000000000000000 ) ) ;
#10201 = FILL_AREA_STYLE_COLOUR ( '', #8866 ) ;
#10202 = CARTESIAN_POINT ( 'NONE',  ( -126.4213562373094959, -6.000000000000000000, 2.255140518769849223E-14 ) ) ;
#10203 = CARTESIAN_POINT ( 'NONE',  ( -795.0000000000080718, 93.55451860843929524, -152.5758913445291398 ) ) ;
#10204 = CARTESIAN_POINT ( 'NONE',  ( 35.00000000000000000, 81.99999999999998579, 190.3192290001959748 ) ) ;
#10205 = EDGE_LOOP ( 'NONE', ( #4815, #4005, #4838, #7609 ) ) ;
#10206 = CARTESIAN_POINT ( 'NONE',  ( -141.4213562373095101, -492.9999999999998863, 3.644282033693712520E-14 ) ) ;
#10207 = CARTESIAN_POINT ( 'NONE',  ( -30.00000000000000000, -492.9999999999998863, -30.00000000000000000 ) ) ;
#10208 = CARTESIAN_POINT ( 'NONE',  ( -383.2280749472602679, 93.16617163057104278, -141.2766522578266404 ) ) ;
#10209 = VERTEX_POINT ( 'NONE', #4464 ) ;
#10210 = CARTESIAN_POINT ( 'NONE',  ( -1024.641217300042399, 73.20632742167555307, -152.5758913445296230 ) ) ;
#10211 = VECTOR ( 'NONE', #2019, 1000.000000000000000 ) ;
#10212 = LINE ( 'NONE', #1749, #6749 ) ;
#10213 = EDGE_LOOP ( 'NONE', ( #5411, #8177, #7633, #447 ) ) ;
#10214 = ORIENTED_EDGE ( 'NONE', *, *, #542, .F. ) ;
#10215 = CARTESIAN_POINT ( 'NONE',  ( -20.00000000000000000, 197.0000000000000000, -124.6807709998038405 ) ) ;
#10216 = AXIS2_PLACEMENT_3D ( 'NONE', #299, #11744, #5988 ) ;
#10217 = ORIENTED_EDGE ( 'NONE', *, *, #11888, .F. ) ;
#10218 = CIRCLE ( 'NONE', #5869, 0.5999999999999998668 ) ;
#10219 = CARTESIAN_POINT ( 'NONE',  ( -380.6759376891203601, 64.70238119921620523, -134.7256802324791636 ) ) ;
#10220 = CARTESIAN_POINT ( 'NONE',  ( 1.249585401188644101E-12, 152.0000000000000000, -6.421356237309483461 ) ) ;
#10221 = DIRECTION ( 'NONE',  ( 1.000000000000000000, 0.000000000000000000, 0.000000000000000000 ) ) ;
#10222 = ORIENTED_EDGE ( 'NONE', *, *, #6177, .F. ) ;
#10223 = CARTESIAN_POINT ( 'NONE',  ( 0.000000000000000000, -58.00000000000000711, -126.4213562373094959 ) ) ;
#10224 = COLOUR_RGB ( '', 0.66274510, 0.83137255, 0.94901961) ;
#10225 = EDGE_CURVE ( 'NONE', #3523, #6435, #4009, .T. ) ;
#10226 = CARTESIAN_POINT ( 'NONE',  ( 1.387778780781445676E-14, 11.99999999999999645, 126.4213562373094959 ) ) ;
#10227 = CARTESIAN_POINT ( 'NONE',  ( 19.98507655485050094, 179.1352618259597307, -125.7279253762596483 ) ) ;
#10228 = EDGE_CURVE ( 'NONE', #3468, #966, #9218, .T. ) ;
#10229 = CARTESIAN_POINT ( 'NONE',  ( -1023.463303304735291, 92.47874188371200432, -95.06748246948023962 ) ) ;
#10230 = LINE ( 'NONE', #4487, #12080 ) ;
#10231 = DIRECTION ( 'NONE',  ( 0.000000000000000000, 0.000000000000000000, 1.000000000000000000 ) ) ;
#10232 = CARTESIAN_POINT ( 'NONE',  ( -928.4368846968637854, 59.55532739646334051, -126.6442663926292056 ) ) ;
#10233 = CIRCLE ( 'NONE', #7672, 7.500000000000007105 ) ;
#10234 = ORIENTED_EDGE ( 'NONE', *, *, #3803, .F. ) ;
#10235 = AXIS2_PLACEMENT_3D ( 'NONE', #11983, #9941, #4271 ) ;
#10236 = FACE_OUTER_BOUND ( 'NONE', #2137, .T. ) ;
#10237 = DIRECTION ( 'NONE',  ( 0.000000000000000000, -1.000000000000000000, 0.000000000000000000 ) ) ;
#10238 = CARTESIAN_POINT ( 'NONE',  ( -370.0269349526453198, 107.9136251528400265, -119.7614542792374408 ) ) ;
#10239 = DIRECTION ( 'NONE',  ( 0.000000000000000000, 1.000000000000000000, 0.000000000000000000 ) ) ;
#10240 = CARTESIAN_POINT ( 'NONE',  ( -928.1401715908999677, 69.16346707076998257, -103.3307627799636919 ) ) ;
#10241 = DIRECTION ( 'NONE',  ( 0.000000000000000000, -1.189524669241239115E-16, 1.000000000000000000 ) ) ;
#10242 = DIRECTION ( 'NONE',  ( 1.000000000000000000, 0.000000000000000000, 0.000000000000000000 ) ) ;
#10243 = CARTESIAN_POINT ( 'NONE',  ( 21.06656027035116807, 179.5228220458012629, -126.2633464264420695 ) ) ;
#10244 = AXIS2_PLACEMENT_3D ( 'NONE', #10678, #10620, #5739 ) ;
#10245 = AXIS2_PLACEMENT_3D ( 'NONE', #9570, #6041, #4007 ) ;
#10246 = CYLINDRICAL_SURFACE ( 'NONE', #9667, 5.000000000000004441 ) ;
#10247 = CARTESIAN_POINT ( 'NONE',  ( -19.98529084832767566, 177.9024039722029613, -123.8679874905754161 ) ) ;
#10248 = CARTESIAN_POINT ( 'NONE',  ( 2.186774452080127126E-12, 12.00000000000000000, 83.57864376269050410 ) ) ;
#10249 = EDGE_CURVE ( 'NONE', #1735, #8803, #9216, .T. ) ;
#10250 = ORIENTED_EDGE ( 'NONE', *, *, #3155, .F. ) ;
#10251 = ORIENTED_EDGE ( 'NONE', *, *, #307, .T. ) ;
#10252 = CARTESIAN_POINT ( 'NONE',  ( -371.3024966496543584, 59.54890786220743593, -140.2366040927702784 ) ) ;
#10253 = CARTESIAN_POINT ( 'NONE',  ( -371.6804198345414534, 103.3022927311476877, -107.1440333209211815 ) ) ;
#10254 = VERTEX_POINT ( 'NONE', #4532 ) ;
#10255 = CARTESIAN_POINT ( 'NONE',  ( -1011.211222789223370, 114.9684118750912489, -107.9061927053323870 ) ) ;
#10256 = PRODUCT_DEFINITION ( 'UNKNOWN', '', #9991, #2825 ) ;
#10257 = CARTESIAN_POINT ( 'NONE',  ( -20.77482174596494247, 180.9926187296578348, -123.5402880645763730 ) ) ;
#10258 = CARTESIAN_POINT ( 'NONE',  ( 21.05508193123089100, 181.5508406828318471, -125.5707457972380325 ) ) ;
#10259 = ORIENTED_EDGE ( 'NONE', *, *, #5332, .F. ) ;
#10260 = AXIS2_PLACEMENT_3D ( 'NONE', #5123, #9753, #1298 ) ;
#10261 = VECTOR ( 'NONE', #8757, 1000.000000000000000 ) ;
#10262 = ORIENTED_EDGE ( 'NONE', *, *, #10556, .T. ) ;
#10263 = ADVANCED_FACE ( 'NONE', ( #11966, #11486 ), #10111, .F. ) ;
#10264 = CARTESIAN_POINT ( 'NONE',  ( 1.874378101782966050E-12, 12.00000000000000000, 53.57864376269050410 ) ) ;
#10265 = CARTESIAN_POINT ( 'NONE',  ( 21.06306891294164529, 179.9350108970479596, -126.4083702064951211 ) ) ;
#10266 = CARTESIAN_POINT ( 'NONE',  ( -853.4539021257704690, 72.48584973916007357, -154.8742214401226818 ) ) ;
#10267 = CARTESIAN_POINT ( 'NONE',  ( -370.3453975627718933, 107.0997924316958176, -115.8836695100632994 ) ) ;
#10268 = FACE_OUTER_BOUND ( 'NONE', #493, .T. ) ;
#10269 = CYLINDRICAL_SURFACE ( 'NONE', #673, 20.00000000000017053 ) ;
#10270 = VERTEX_POINT ( 'NONE', #8994 ) ;
#10271 = CARTESIAN_POINT ( 'NONE',  ( 0.000000000000000000, -6.000000000000000000, 0.000000000000000000 ) ) ;
#10272 = CARTESIAN_POINT ( 'NONE',  ( -383.3150907383348454, 92.89194869614372863, -141.4579310800400549 ) ) ;
#10273 = VERTEX_POINT ( 'NONE', #11967 ) ;
#10274 = CARTESIAN_POINT ( 'NONE',  ( -1019.723937646960849, 86.79129919622100431, -154.8742214401232502 ) ) ;
#10275 = EDGE_LOOP ( 'NONE', ( #2637, #10195, #5329, #10326 ) ) ;
#10276 = ORIENTED_EDGE ( 'NONE', *, *, #11879, .T. ) ;
#10277 = CARTESIAN_POINT ( 'NONE',  ( -1057.521967982373098, 48.25222617153974625, -141.4553492942758623 ) ) ;
#10278 = ORIENTED_EDGE ( 'NONE', *, *, #5015, .T. ) ;
#10279 = CARTESIAN_POINT ( 'NONE',  ( -372.1640597400288470, 62.26788882665526614, -144.4898947985778079 ) ) ;
#10280 = CARTESIAN_POINT ( 'NONE',  ( 151.3258811035896656, 0.000000000000000000, -48.63263083939796871 ) ) ;
#10281 = CARTESIAN_POINT ( 'NONE',  ( -141.4213562373095101, -494.9999999999998863, 3.644282033693712520E-14 ) ) ;
#10282 = VERTEX_POINT ( 'NONE', #1459 ) ;
#10283 = DIRECTION ( 'NONE',  ( -8.163404592832030268E-17, 1.000000000000000000, -0.000000000000000000 ) ) ;
#10284 = B_SPLINE_SURFACE_WITH_KNOTS ( 'NONE', 3, 3, ( 
 ( #6851, #10616, #3823, #989, #2904, #5854, #11427, #4929, #7597, #1115, #3762, #2843, #4986, #9689, #8708, #4867, #9511, #9628, #7712, #2960 ),
 ( #11365, #7536, #11304, #6609, #1979, #6723, #8530, #4010, #6668, #8652, #2159, #5922, #1175, #10499, #1056, #5791, #7778, #1232, #3021, #9572 ),
 ( #4814, #8587, #10371, #109, #3137, #9810, #9994, #10738, #7027, #10917, #8025, #4075, #7907, #8931, #7844, #11618, #10674, #1293, #1465, #464 ),
 ( #8086, #7152, #4188, #3193, #1350, #5114, #11736, #2338, #6107, #2450, #8518, #6771, #6656, #10487, #214, #1163, #3936, #8574, #5724, #3872 ),
 ( #5844, #4856, #98, #5778, #1041, #7644, #5604, #3996, #8468, #11413, #3068, #9557, #1103, #11541, #8637, #1840, #3011, #4694, #6837, #12230 ),
 ( #5205, #4299, #1444, #10786, #8068, #272, #3123, #2262, #5097, #4063, #10606, #10664, #7828, #1337, #6033, #4121, #8813, #2144, #6895, #9797 ),
 ( #1217, #1278, #7895, #11603, #9679, #443, #5909, #3351, #8981, #3236, #2201, #5968, #512, #5036, #9860, #3179, #11840, #8756, #11662, #9736 ),
 ( #1391, #335, #6956, #10724, #4975, #8868, #393, #4172, #7949, #11721, #7015, #2323, #6092, #5153, #8915, #4236, #8010, #11780, #3296, #7071 ),
 ( #10842, #2376, #6147, #9915, #11028, #6328, #6455, #10229, #7197, #9043, #10042, #5458, #2558, #12087, #7326, #11091, #1509, #9234, #1765, #5270 ),
 ( #7133, #2493, #2430, #1572, #4548, #6211, #5526, #842, #9300, #2616, #4614, #581, #11891, #10099, #1632, #4358, #10899, #10966, #8128, #5393 ),
 ( #643, #5333, #9979, #3406, #9172, #6270, #9104, #4418, #8195, #11958, #3474, #776, #4485, #12156, #8258, #12017, #3533, #6392, #10163, #1698 ),
 ( #8324, #3598, #7387, #11158, #2684, #4790, #11280, #10528, #10406, #10473, #2993, #7689, #8558, #2008, #9542, #1947, #12212, #5652, #3920, #15 ),
 ( #6520, #9426, #5764, #11335, #962, #8620, #10287, #4676, #1890, #8506, #2876, #4734, #2070, #2752, #3792, #6641, #5708, #7566, #9483, #7444 ),
 ( #5827, #79, #1021, #3857, #9605, #7630, #1088, #6582, #11399, #2936, #11462, #5589, #6754, #9365, #1827, #6699, #910, #4842, #137, #1148 ),
 ( #8454, #3735, #7509, #2811, #10346, #4900, #8686, #3671, #11226, #2246, #7813, #11709, #10650, #11522, #10590, #3979, #1205, #7748, #2188, #10830 ),
 ( #5142, #3051, #3223, #11587, #7999, #5889, #317, #11647, #11768, #3283, #257, #2131, #3108, #10770, #4105, #8903, #4047, #1320, #194, #6821 ),
 ( #9903, #430, #5080, #5954, #6077, #4162, #7877, #9666, #6881, #4962, #8740, #5196, #9722, #6940, #1259, #4220, #5020, #8855, #2369, #7058 ),
 ( #10709, #8798, #6015, #9844, #6136, #7000, #9781, #7936, #3166, #382, #2307, #1437, #1379, #5592, #7632, #9368, #912, #8561, #5654, #10166 ),
 ( #1700, #9303, #3795, #5461, #1025, #82, #9485, #10349, #3859, #8327, #6458, #4678, #8456, #12089, #4552, #10232, #1768, #12214, #3738, #7512 ),
 ( #5528, #11282, #2814, #9429, #964, #4737, #7568, #11337, #2879, #10409, #1950, #9544, #8623, #11589, #7691, #6756, #139, #5829, #5957, #7751 ),
 ( #2072, #11524, #1150, #8689, #320, #6824, #10592, #5892, #9669, #6018, #259, #6883, #3168, #6943, #8377, #3657, #3725, #5698, #764, #8316 ),
 ( #2739, #6507, #10277, #11326, #9352, #11271, #6571, #1878, #5641, #9415, #950, #9471, #11573, #4030, #2980, #7802, #4949, #8675, #6871, #4832 ),
 ( #9655, #5754, #9530, #3158, #7679, #3101, #9592, #2233, #2924, #2053, #1074, #8609, #10640, #129, #6686, #3905, #3846, #7865, #5814, #10462 ),
 ( #6741, #1137, #4887, #8727, #8549, #11449, #67, #10519, #6931, #7620, #9713, #11387, #2179, #182, #309, #1996, #3965, #7734, #4095, #11639 ),
 ( #11508, #3037, #5941, #6807, #1251, #10579, #5875, #4778, #2117, #9770, #6000, #5006, #1197, #245, #8785, #10696, #485, #11694, #11757, #5065 ),
 ( #8843, #2358, #11812, #9827, #6246, #3328, #2407, #2527, #614, #3381, #7108, #3209, #10871, #10014, #5305, #4332, #6184, #9014, #9950, #1488 ),
 ( #9078, #6985, #8102, #10758, #4389, #8162, #2291, #6060, #1367, #5428, #5362, #743, #7482, #9140, #4707, #3768, #935, #10266, #3566, #3705 ),
 ( #1740, #679, #9207, #1601, #4454, #2847, #12054, #4585, #6360, #2785, #4521, #11199, #8484, #9399, #12190, #8359, #11992, #12125, #6550, #1859 ),
 ( #3636, #1797, #8299, #6429, #8232, #10317, #3507, #7357, #11309, #11127, #7421, #5238, #5561, #10070, #2652, #7299, #10199, #5621, #11063, #7541 ),
 ( #2588, #9336, #10132, #1666, #5501, #9274, #2721, #813, #6491, #877, #4649, #8425, #2038, #113, #8591, #10378, #11371, #5796, #9457, #995 ),
 ( #3891, #3827, #5680, #8713, #1918, #6614, #4992, #11494, #7602, #2911, #8772, #9516, #5859, #11432, #7849, #4760, #7662, #6673, #10443, #9634 ),
 ( #1119, #1182, #5927, #10621, #6789, #4935, #229, #8658, #1983, #2965, #6858, #6727, #8535, #50, #10503, #4016, #9579, #169, #11559, #5740 ),
 ( #3951, #7717, #10563, #2106, #293, #1060, #7783, #3085, #2166, #9695, #2012, #2757, #9546, #4681, #8457, #10308, #11115, #6601, #4440, #11094 ),
 ( #3132, #1001, #60, #6905, #7903, #11673, #3187, #6963, #4769, #2916, #10452, #8875, #11729, #3244, #1226, #6104, #1402, #7839, #456, #1809 ),
 ( #825, #1002, #5634, #940, #4876, #2852, #361, #4145, #410, #9885, #234, #4020, #7788, #1242, #6863, #2349, #8036, #1416, #3318, #7917 ),
 ( #1359, #300, #1186, #11566, #9820, #5127, #3093, #4199, #5179, #10630, #2171, #8940, #6977, #7100, #11682, #10748, #4941, #6119, #3148, #11802 ) ),
 .UNSPECIFIED., .T., .F., .F.,
 ( 4, 1, 1, 1, 1, 1, 1, 1, 1, 1, 1, 1, 1, 1, 1, 1, 2, 1, 1, 1, 1, 1, 1, 1, 1, 1, 1, 1, 1, 1, 1, 1, 4 ),
 ( 4, 1, 1, 1, 2, 1, 1, 1, 2, 2, 2, 2, 4 ),
 ( 0.000000000000000000, 0.03125000000000000000, 0.06250000000000000000, 0.09375000000000000000, 0.1250000000000000000, 0.1562500000000000000, 0.1875000000000000000, 0.2187500000000000000, 0.2500000000000000000, 0.2812500000000000000, 0.3125000000000000000, 0.3437500000000000000, 0.3750000000000000000, 0.4062500000000000000, 0.4375000000000000000, 0.4687500000000000000, 0.5000000000000000000, 0.5312500000000000000, 0.5625000000000000000, 0.5937500000000000000, 0.6250000000000000000, 0.6562500000000000000, 0.6875000000000000000, 0.7187500000000000000, 0.7500000000000000000, 0.7812500000000000000, 0.8125000000000000000, 0.8437500000000000000, 0.8750000000000000000, 0.9062500000000000000, 0.9375000000000000000, 0.9687500000000000000, 1.000000000000000000 ),
 ( 0.000000000000000000, 0.04762575996673557022, 0.07143863995010346635, 0.09525151993347125146, 0.1428772799002068217, 0.1647615404280894369, 0.1757036706920307445, 0.1866458009559719411, 0.2085300614838545563, 0.4016963878702066726, 0.4307237013227157574, 0.6771470142487683308, 1.000000000000000000 ),
 .UNSPECIFIED. ) ;
#10285 = DIRECTION ( 'NONE',  ( 0.000000000000000000, 0.000000000000000000, 1.000000000000000000 ) ) ;
#10286 = CARTESIAN_POINT ( 'NONE',  ( 19.97135992617064915, 177.8754454934489218, -125.7601421070351222 ) ) ;
#10287 = CARTESIAN_POINT ( 'NONE',  ( -1027.708477481198088, 65.70736702952430619, -99.57582448894528682 ) ) ;
#10288 = CARTESIAN_POINT ( 'NONE',  ( 6.500000000000030198, -6.999999999999977796, -124.6807709998038405 ) ) ;
#10289 = EDGE_LOOP ( 'NONE', ( #4566, #11328 ) ) ;
#10290 = CARTESIAN_POINT ( 'NONE',  ( 35.00000000000000000, 163.9999999999999716, 190.3192290001959748 ) ) ;
#10291 = ADVANCED_FACE ( 'NONE', ( #10978 ), #11904, .F. ) ;
#10292 = DIRECTION ( 'NONE',  ( 0.03251933543158296025, -4.204120722334267754E-17, 0.9994711065474020106 ) ) ;
#10293 = CARTESIAN_POINT ( 'NONE',  ( -150.0000000000000000, 139.9999999999999716, -126.4213562373084301 ) ) ;
#10294 = ORIENTED_EDGE ( 'NONE', *, *, #7842, .T. ) ;
#10295 = AXIS2_PLACEMENT_3D ( 'NONE', #7775, #1292, #4985 ) ;
#10297 = ADVANCED_FACE ( 'NONE', ( #7271, #11039 ), #8273, .F. ) ;
#10296 = CARTESIAN_POINT ( 'NONE',  ( -954.0832773815070595, 60.15510303592672869, -103.3307627799632513 ) ) ;
#10298 = DIRECTION ( 'NONE',  ( 0.000000000000000000, -1.000000000000000000, -4.625929269271452387E-16 ) ) ;
#10299 = LINE ( 'NONE', #6529, #2833 ) ;
#10300 = CYLINDRICAL_SURFACE ( 'NONE', #9902, 35.00000000000000000 ) ;
#10301 = DIRECTION ( 'NONE',  ( 0.000000000000000000, 1.632680918566399772E-14, -1.000000000000000000 ) ) ;
#10302 = CARTESIAN_POINT ( 'NONE',  ( -20.98196205190248875, 178.7079620517401963, -124.7263650620788269 ) ) ;
#10303 = FACE_OUTER_BOUND ( 'NONE', #2598, .T. ) ;
#10304 = AXIS2_PLACEMENT_3D ( 'NONE', #10424, #4691, #856 ) ;
#10305 = ORIENTED_EDGE ( 'NONE', *, *, #11161, .T. ) ;
#10306 = CARTESIAN_POINT ( 'NONE',  ( -374.2311861953731977, 71.64084721860098171, -152.2531916975700881 ) ) ;
#10307 = CARTESIAN_POINT ( 'NONE',  ( -382.8879895414342514, 94.18609904179986358, -108.8085965833891890 ) ) ;
#10308 = CARTESIAN_POINT ( 'NONE',  ( -926.5908784743301112, 123.4113341959662762, -136.2353035311976441 ) ) ;
#10309 = ORIENTED_EDGE ( 'NONE', *, *, #10564, .T. ) ;
#10310 = CARTESIAN_POINT ( 'NONE',  ( -1037.461794897084019, 110.6138330393709879, -107.9061927053326144 ) ) ;
#10311 = CARTESIAN_POINT ( 'NONE',  ( -180.0000000000000000, 151.9999999999999716, -126.4213562373082453 ) ) ;
#10312 = EDGE_CURVE ( 'NONE', #3344, #9710, #3682, .T. ) ;
#10313 = CARTESIAN_POINT ( 'NONE',  ( 19.97825765123714348, 180.7277658390849808, -126.0785619755266822 ) ) ;
#10314 = ORIENTED_EDGE ( 'NONE', *, *, #5082, .T. ) ;
#10315 = DIRECTION ( 'NONE',  ( 0.000000000000000000, 0.000000000000000000, -1.000000000000000000 ) ) ;
#10316 = DIRECTION ( 'NONE',  ( -0.3117078928809153826, -1.979053562451413181E-14, -0.9501779778103363050 ) ) ;
#10317 = CARTESIAN_POINT ( 'NONE',  ( -1031.476138302183244, 95.34216976508434982, -152.5758913445290830 ) ) ;
#10318 = CARTESIAN_POINT ( 'NONE',  ( -379.6261022631920810, 101.2176309556962082, -119.1318278414791507 ) ) ;
#10319 = AXIS2_PLACEMENT_3D ( 'NONE', #2742, #5582, #9356 ) ;
#10320 = CYLINDRICAL_SURFACE ( 'NONE', #1178, 7.500000000000007994 ) ;
#10321 = CARTESIAN_POINT ( 'NONE',  ( 4.454233577106967753E-15, 166.0000000000000000, -124.6807709998038405 ) ) ;
#10322 = DIRECTION ( 'NONE',  ( 3.061276722312011504E-17, -1.000000000000000000, 0.000000000000000000 ) ) ;
#10323 = ORIENTED_EDGE ( 'NONE', *, *, #3282, .F. ) ;
#10324 = FACE_OUTER_BOUND ( 'NONE', #12069, .T. ) ;
#10325 = CARTESIAN_POINT ( 'NONE',  ( -373.6516460492721308, 96.99228658101947076, -138.0176360913489191 ) ) ;
#10326 = ORIENTED_EDGE ( 'NONE', *, *, #8797, .F. ) ;
#10327 = EDGE_CURVE ( 'NONE', #9573, #10254, #11208, .T. ) ;
#10328 = CARTESIAN_POINT ( 'NONE',  ( -853.4539021257704690, 72.48584973916007357, -154.8742214401226818 ) ) ;
#10329 = VECTOR ( 'NONE', #6405, 1000.000000000000000 ) ;
#10330 = EDGE_CURVE ( 'NONE', #1813, #3290, #607, .T. ) ;
#10331 = VERTEX_POINT ( 'NONE', #4230 ) ;
#10332 = VERTEX_POINT ( 'NONE', #507 ) ;
#10333 = CARTESIAN_POINT ( 'NONE',  ( -375.0000000000000000, 81.99999999999995737, -89.68077099980384048 ) ) ;
#10334 = CARTESIAN_POINT ( 'NONE',  ( 0.000000000000000000, 0.000000000000000000, -118.9213562373094817 ) ) ;
#10335 = FACE_BOUND ( 'NONE', #2047, .T. ) ;
#10336 = TOROIDAL_SURFACE ( 'NONE', #10139, 8.500000000000007105, 1.000000000000000000 ) ;
#10337 = ORIENTED_EDGE ( 'NONE', *, *, #1462, .T. ) ;
#10338 = CARTESIAN_POINT ( 'NONE',  ( -382.8924036478341009, 69.79657916374794979, -140.5797354247098099 ) ) ;
#10339 = PLANE ( 'NONE',  #12102 ) ;
#10340 = CARTESIAN_POINT ( 'NONE',  ( -374.2594319682045807, 70.51193190803552113, -108.2281409940259351 ) ) ;
#10341 = DIRECTION ( 'NONE',  ( 0.000000000000000000, 0.000000000000000000, -1.000000000000000000 ) ) ;
#10342 = ORIENTED_EDGE ( 'NONE', *, *, #12116, .T. ) ;
#10343 = VECTOR ( 'NONE', #9470, 1000.000000000000000 ) ;
#10344 = AXIS2_PLACEMENT_3D ( 'NONE', #2929, #2983, #9475 ) ;
#10345 = DIRECTION ( 'NONE',  ( -0.000000000000000000, 1.000000000000000000, 0.000000000000000000 ) ) ;
#10346 = CARTESIAN_POINT ( 'NONE',  ( -1038.595419435790973, 46.89684673038605922, -107.9061927053327850 ) ) ;
#10347 = CARTESIAN_POINT ( 'NONE',  ( -818.8602300167407293, 79.32305858693317191, -104.8581405595893727 ) ) ;
#10348 = DIRECTION ( 'NONE',  ( -8.163404592832030268E-17, 1.000000000000000000, -0.000000000000000000 ) ) ;
#10349 = CARTESIAN_POINT ( 'NONE',  ( -1025.976186494711783, 52.68972726728017619, -126.6442663926293193 ) ) ;
#10350 = EDGE_LOOP ( 'NONE', ( #6944, #10214 ) ) ;
#10351 = AXIS2_PLACEMENT_3D ( 'NONE', #3506, #11126, #3635 ) ;
#10352 = FACE_BOUND ( 'NONE', #2010, .T. ) ;
#10353 = CIRCLE ( 'NONE', #5803, 7.500000000000007105 ) ;
#10354 = DIRECTION ( 'NONE',  ( 0.000000000000000000, -1.000000000000000000, 0.000000000000000000 ) ) ;
#10355 = CARTESIAN_POINT ( 'NONE',  ( -373.4608161113892493, 96.60585252165465420, -99.74601397596084951 ) ) ;
#10356 = ORIENTED_EDGE ( 'NONE', *, *, #2029, .F. ) ;
#10357 = CARTESIAN_POINT ( 'NONE',  ( -1013.844210246976672, 57.79547239392030633, -107.9061927053327423 ) ) ;
#10358 = CARTESIAN_POINT ( 'NONE',  ( -37.49999999999999289, -9.213203435596451385, -126.4213562373092685 ) ) ;
#10359 = DIRECTION ( 'NONE',  ( 0.000000000000000000, 0.000000000000000000, -1.000000000000000000 ) ) ;
#10360 = CARTESIAN_POINT ( 'NONE',  ( 19.83206362640841647, 180.0177979251707825, -127.2672250451624905 ) ) ;
#10361 = ADVANCED_FACE ( 'NONE', ( #3401 ), #8019, .F. ) ;
#10362 = CIRCLE ( 'NONE', #9581, 7.500000000000007105 ) ;
#10363 = FACE_BOUND ( 'NONE', #2938, .T. ) ;
#10364 = ORIENTED_EDGE ( 'NONE', *, *, #9947, .F. ) ;
#10365 = CARTESIAN_POINT ( 'NONE',  ( 6.899999999999999467, 7.794228634059940042, 4.500000000000007105 ) ) ;
#10366 = ORIENTED_EDGE ( 'NONE', *, *, #9392, .T. ) ;
#10367 = CARTESIAN_POINT ( 'NONE',  ( -954.1708249681036023, 122.1961423320943680, -113.1262384684093263 ) ) ;
#10368 = AXIS2_PLACEMENT_3D ( 'NONE', #10805, #5929, #10744 ) ;
#10369 = DIRECTION ( 'NONE',  ( 0.000000000000000000, 0.000000000000000000, -1.000000000000000000 ) ) ;
#10370 = DIRECTION ( 'NONE',  ( -0.000000000000000000, 1.000000000000000000, 7.930164461608263644E-17 ) ) ;
#10371 = CARTESIAN_POINT ( 'NONE',  ( -1054.407929976941432, 113.5897173251036207, -118.7903414690678261 ) ) ;
#10372 = VERTEX_POINT ( 'NONE', #10792 ) ;
#10373 = ADVANCED_FACE ( 'NONE', ( #5218 ), #524, .T. ) ;
#10374 = DIRECTION ( 'NONE',  ( 0.000000000000000000, 0.000000000000000000, 1.000000000000000000 ) ) ;
#10375 = EDGE_CURVE ( 'NONE', #1167, #6680, #10911, .T. ) ;
#10376 = FACE_OUTER_BOUND ( 'NONE', #7186, .T. ) ;
#10377 = CARTESIAN_POINT ( 'NONE',  ( 0.000000000000000000, 0.000000000000000000, 5.999999999999999112 ) ) ;
#10378 = CARTESIAN_POINT ( 'NONE',  ( -926.9570750291560444, 111.1083136274932031, -149.7857175106636021 ) ) ;
#10379 = FILL_AREA_STYLE ('',( #2039 ) ) ;
#10380 = DIRECTION ( 'NONE',  ( -1.000000000000000000, 0.000000000000000000, 0.000000000000000000 ) ) ;
#10381 = VERTEX_POINT ( 'NONE', #1517 ) ;
#10382 = EDGE_CURVE ( 'NONE', #90, #2078, #5341, .T. ) ;
#10383 = PRODUCT_DEFINITION_SHAPE ( 'NONE', 'NONE',  #9348 ) ;
#10384 = ORIENTED_EDGE ( 'NONE', *, *, #7505, .T. ) ;
#10385 = CARTESIAN_POINT ( 'NONE',  ( -1065.000000000002956, 76.10956187831469322, -154.2940595301282087 ) ) ;
#10386 = PRODUCT_DEFINITION_FORMATION_WITH_SPECIFIED_SOURCE ( 'ANY', '', #6637, .NOT_KNOWN. ) ;
#10387 = DIRECTION ( 'NONE',  ( 1.000000000000000000, 0.000000000000000000, -0.000000000000000000 ) ) ;
#10388 = AXIS2_PLACEMENT_3D ( 'NONE', #10472, #9665, #4731 ) ;
#10389 = CARTESIAN_POINT ( 'NONE',  ( -819.8566349279940368, 81.72907896098652714, -154.3841807065155933 ) ) ;
#10390 = ORIENTED_EDGE ( 'NONE', *, *, #5684, .T. ) ;
#10391 = CARTESIAN_POINT ( 'NONE',  ( 0.000000000000000000, 0.000000000000000000, -124.6807709998040110 ) ) ;
#10392 = CARTESIAN_POINT ( 'NONE',  ( -824.5038201930772175, 73.70910806073493404, -106.4800466717826595 ) ) ;
#10393 = EDGE_LOOP ( 'NONE', ( #2805, #9341, #4450, #9326 ) ) ;
#10394 = EDGE_CURVE ( 'NONE', #7119, #3163, #6068, .T. ) ;
#10395 = CARTESIAN_POINT ( 'NONE',  ( -382.4233354741761559, 68.57082533223261578, -139.5051951744822816 ) ) ;
#10396 = CARTESIAN_POINT ( 'NONE',  ( 7.500000000000000000, 5.196152422706624030, -9.000000000000000000 ) ) ;
#10397 = CARTESIAN_POINT ( 'NONE',  ( -374.3220111056598967, 72.27247505761226876, -96.81229118638817965 ) ) ;
#10398 = AXIS2_PLACEMENT_3D ( 'NONE', #10226, #11089, #9232 ) ;
#10399 = CARTESIAN_POINT ( 'NONE',  ( 0.000000000000000000, 0.000000000000000000, 0.000000000000000000 ) ) ;
#10400 = ORIENTED_EDGE ( 'NONE', *, *, #10450, .F. ) ;
#10401 = EDGE_CURVE ( 'NONE', #6960, #3617, #6261, .T. ) ;
#10402 = ADVANCED_FACE ( 'NONE', ( #1456 ), #738, .T. ) ;
#10403 = DIRECTION ( 'NONE',  ( 0.000000000000000000, 1.000000000000000000, 0.000000000000000000 ) ) ;
#10404 = DIRECTION ( 'NONE',  ( 1.000000000000000000, 0.000000000000000000, 0.000000000000000000 ) ) ;
#10405 = CIRCLE ( 'NONE', #8645, 7.500000000000007105 ) ;
#10406 = CARTESIAN_POINT ( 'NONE',  ( -1020.430183747026263, 74.13649791779302234, -96.78565065507955012 ) ) ;
#10407 = DIRECTION ( 'NONE',  ( -1.000000000000000000, 1.262554838833776231E-16, 0.000000000000000000 ) ) ;
#10408 = CARTESIAN_POINT ( 'NONE',  ( -89.99999999999998579, 12.00000000000001421, -126.4213562373088564 ) ) ;
#10409 = CARTESIAN_POINT ( 'NONE',  ( -1017.133222628203043, 54.07990892584120246, -130.5712005305404375 ) ) ;
#10410 = EDGE_CURVE ( 'NONE', #9092, #5919, #2238, .T. ) ;
#10411 = DIRECTION ( 'NONE',  ( -8.163404592832030268E-17, 1.000000000000000000, -0.000000000000000000 ) ) ;
#10412 = ORIENTED_EDGE ( 'NONE', *, *, #3295, .F. ) ;
#10413 = CARTESIAN_POINT ( 'NONE',  ( -821.6112282492910026, 83.16771792585103640, -144.6470480974979864 ) ) ;
#10414 = APPLICATION_PROTOCOL_DEFINITION ( 'draft international standard', 'automotive_design', 1998, #10713 ) ;
#10415 = CARTESIAN_POINT ( 'NONE',  ( -369.9264633483897455, 108.1643382291179449, -122.0075474512173059 ) ) ;
#10416 = FACE_OUTER_BOUND ( 'NONE', #11322, .T. ) ;
#10417 = VERTEX_POINT ( 'NONE', #5331 ) ;
#10418 = CARTESIAN_POINT ( 'NONE',  ( -853.9759289228104535, 31.63339360934237021, -107.9061927053328986 ) ) ;
#10419 = AXIS2_PLACEMENT_3D ( 'NONE', #2123, #9775, #6993 ) ;
#10420 = FACE_OUTER_BOUND ( 'NONE', #5176, .T. ) ;
#10421 = CARTESIAN_POINT ( 'NONE',  ( -120.8820948793972434, 12.00000000000000000, -186.6989091883324363 ) ) ;
#10422 = DIRECTION ( 'NONE',  ( 0.000000000000000000, -1.000000000000000000, 0.000000000000000000 ) ) ;
#10423 = DIRECTION ( 'NONE',  ( 0.000000000000000000, -1.000000000000000000, 0.000000000000000000 ) ) ;
#10424 = CARTESIAN_POINT ( 'NONE',  ( 7.347064133548826625E-16, 139.9999999999999716, -126.4213562373094959 ) ) ;
#10425 = DIRECTION ( 'NONE',  ( 3.061276722312011504E-17, -1.000000000000000000, 0.000000000000000000 ) ) ;
#10426 = CYLINDRICAL_SURFACE ( 'NONE', #2851, 8.999999999999998224 ) ;
#10427 = CIRCLE ( 'NONE', #3126, 1.000000000000000888 ) ;
#10428 = ORIENTED_EDGE ( 'NONE', *, *, #9425, .F. ) ;
#10429 = CARTESIAN_POINT ( 'NONE',  ( -6.097041784444755962E-13, 12.00000000000000000, -237.1807709998039115 ) ) ;
#10430 = CARTESIAN_POINT ( 'NONE',  ( -381.7638695068005745, 97.03891058473890041, -111.4316689550042270 ) ) ;
#10431 = ORIENTED_EDGE ( 'NONE', *, *, #1258, .F. ) ;
#10432 = CARTESIAN_POINT ( 'NONE',  ( -974.4564103291414767, 111.0951925441806480, -103.3307627799632371 ) ) ;
#10433 = AXIS2_PLACEMENT_3D ( 'NONE', #12029, #7458, #2697 ) ;
#10434 = LINE ( 'NONE', #3817, #10794 ) ;
#10435 = LINE ( 'NONE', #2712, #5284 ) ;
#10436 = AXIS2_PLACEMENT_3D ( 'NONE', #6965, #2272, #4865 ) ;
#10437 = CARTESIAN_POINT ( 'NONE',  ( 21.00606259948788335, 181.7116910486332984, -124.9297615680210498 ) ) ;
#10438 = DIRECTION ( 'NONE',  ( 0.000000000000000000, 0.000000000000000000, 1.000000000000000000 ) ) ;
#10439 = EDGE_LOOP ( 'NONE', ( #10617, #10694, #9460, #11502, #3061, #4958 ) ) ;
#10440 = DIRECTION ( 'NONE',  ( 0.000000000000000000, 1.000000000000000000, 0.000000000000000000 ) ) ;
#10441 = VECTOR ( 'NONE', #3141, 1000.000000000000000 ) ;
#10442 = CARTESIAN_POINT ( 'NONE',  ( -7.500000000000000888, 166.0000000000000000, -124.6807709998038405 ) ) ;
#10443 = CARTESIAN_POINT ( 'NONE',  ( -822.7482738817701602, 104.4536172844453148, -146.0307792196443017 ) ) ;
#10444 = CARTESIAN_POINT ( 'NONE',  ( -270.0000000000000000, 151.9999999999999716, -126.4213562373076059 ) ) ;
#10445 = DIRECTION ( 'NONE',  ( 0.000000000000000000, 1.000000000000000000, 0.000000000000000000 ) ) ;
#10446 = CARTESIAN_POINT ( 'NONE',  ( -3.161662739628749519E-15, 267.2792206135785591, -126.4213562373094959 ) ) ;
#10447 = ORIENTED_EDGE ( 'NONE', *, *, #7995, .T. ) ;
#10448 = AXIS2_PLACEMENT_3D ( 'NONE', #3703, #5619, #4758 ) ;
#10449 = DIRECTION ( 'NONE',  ( 0.000000000000000000, 1.000000000000000000, 0.000000000000000000 ) ) ;
#10450 = EDGE_CURVE ( 'NONE', #11532, #7797, #1736, .T. ) ;
#10451 = CARTESIAN_POINT ( 'NONE',  ( -903.6727718957008619, 110.0506089609179838, -149.7857175106632326 ) ) ;
#10452 = CARTESIAN_POINT ( 'NONE',  ( -1010.947924043452645, 120.1731093567702828, -130.5712005305404375 ) ) ;
#10453 = ADVANCED_FACE ( 'NONE', ( #8323 ), #3104, .T. ) ;
#10454 = AXIS2_PLACEMENT_3D ( 'NONE', #10444, #1062, #4819 ) ;
#10455 = CARTESIAN_POINT ( 'NONE',  ( -45.53315400109751465, 0.000000000000000000, -245.3419396193594650 ) ) ;
#10456 = ORIENTED_EDGE ( 'NONE', *, *, #4516, .F. ) ;
#10457 = ORIENTED_EDGE ( 'NONE', *, *, #7214, .T. ) ;
#10458 = EDGE_CURVE ( 'NONE', #83, #1863, #2504, .T. ) ;
#10459 = CARTESIAN_POINT ( 'NONE',  ( 126.4213562373094959, 0.000000000000000000, 7.500000000000006217 ) ) ;
#10460 = CARTESIAN_POINT ( 'NONE',  ( -20.92339290342903979, 181.6071613487999059, -124.3124672736065577 ) ) ;
#10461 = CARTESIAN_POINT ( 'NONE',  ( -818.9891295040824843, 77.37577012656028330, -105.2199448511381235 ) ) ;
#10462 = CARTESIAN_POINT ( 'NONE',  ( -795.0000000000071623, 60.65002596136950075, -146.0307792196447565 ) ) ;
#10463 = ORIENTED_EDGE ( 'NONE', *, *, #8356, .T. ) ;
#10464 = CARTESIAN_POINT ( 'NONE',  ( -384.3557402719069387, 75.23780925246066431, -143.5057597349512264 ) ) ;
#10465 = LINE ( 'NONE', #186, #3615 ) ;
#10466 = CARTESIAN_POINT ( 'NONE',  ( -374.1438204953303739, 71.07787666357693013, -97.39646298909734412 ) ) ;
#10467 = CARTESIAN_POINT ( 'NONE',  ( 144.0488662551573782, 0.000000000000000000, -154.4077238332702393 ) ) ;
#10468 = DIRECTION ( 'NONE',  ( 0.000000000000000000, 0.000000000000000000, 1.000000000000000000 ) ) ;
#10469 = EDGE_CURVE ( 'NONE', #739, #725, #10405, .T. ) ;
#10470 = ORIENTED_EDGE ( 'NONE', *, *, #7613, .T. ) ;
#10471 = EDGE_CURVE ( 'NONE', #6669, #3591, #4483, .T. ) ;
#10472 = CARTESIAN_POINT ( 'NONE',  ( 0.000000000000000000, 12.00000000000000000, -89.68077099980401101 ) ) ;
#10473 = CARTESIAN_POINT ( 'NONE',  ( -1016.123300349496276, 74.17810748283143596, -96.78565065507957854 ) ) ;
#10474 = CARTESIAN_POINT ( 'NONE',  ( -822.6918648528317135, 83.54617135776037173, -104.7406007859487715 ) ) ;
#10475 = DIRECTION ( 'NONE',  ( -0.000000000000000000, -0.000000000000000000, -1.000000000000000000 ) ) ;
#10476 = VERTEX_POINT ( 'NONE', #11157 ) ;
#10477 = CARTESIAN_POINT ( 'NONE',  ( -818.8602280653290109, 79.32430977885860557, -144.5036099591918344 ) ) ;
#10478 = ORIENTED_EDGE ( 'NONE', *, *, #7595, .F. ) ;
#10479 = APPLICATION_PROTOCOL_DEFINITION ( 'draft international standard', 'automotive_design', 1998, #1016 ) ;
#10480 = CARTESIAN_POINT ( 'NONE',  ( -371.6737729595722044, 103.3297310517157115, -107.1558738098986083 ) ) ;
#10481 = VERTEX_POINT ( 'NONE', #2862 ) ;
#10482 = CARTESIAN_POINT ( 'NONE',  ( -1062.493403002516516, 61.99900353997416147, -99.57582448894515892 ) ) ;
#10483 = FACE_OUTER_BOUND ( 'NONE', #650, .T. ) ;
#10484 = DIRECTION ( 'NONE',  ( 1.000000000000000000, 0.000000000000000000, -0.000000000000000000 ) ) ;
#10485 = EDGE_CURVE ( 'NONE', #2611, #9028, #6626, .T. ) ;
#10486 = PRODUCT_DEFINITION_CONTEXT ( 'detailed design', #8448, 'design' ) ;
#10487 = CARTESIAN_POINT ( 'NONE',  ( -954.1708249681036023, 122.1961423320943680, -113.1262384684093263 ) ) ;
#10488 = CARTESIAN_POINT ( 'NONE',  ( 6.899999999999999467, 5.196152422706624030, -9.000000000000000000 ) ) ;
#10489 = CARTESIAN_POINT ( 'NONE',  ( -19.99365627236732834, 178.8147210300960239, -125.2696703636239448 ) ) ;
#10490 = DIRECTION ( 'NONE',  ( 0.000000000000000000, 1.000000000000000000, 0.000000000000000000 ) ) ;
#10491 = AXIS2_PLACEMENT_3D ( 'NONE', #599, #11911, #7217 ) ;
#10492 = ORIENTED_EDGE ( 'NONE', *, *, #9249, .T. ) ;
#10493 = PRODUCT_DEFINITION_SHAPE ( 'NONE', 'NONE',  #9935 ) ;
#10494 = ORIENTED_EDGE ( 'NONE', *, *, #11459, .F. ) ;
#10495 = CARTESIAN_POINT ( 'NONE',  ( -992.5689194452221500, 110.2481211102048491, -103.3307627799634218 ) ) ;
#10496 = CARTESIAN_POINT ( 'NONE',  ( 0.000000000000000000, 164.0000000000000000, -124.6807709998038405 ) ) ;
#10497 = DIRECTION ( 'NONE',  ( -8.163404592832030268E-17, 1.000000000000000000, -0.000000000000000000 ) ) ;
#10498 = CIRCLE ( 'NONE', #8126, 7.500000000000007105 ) ;
#10499 = CARTESIAN_POINT ( 'NONE',  ( -954.0441199534441239, 124.9954171138387977, -122.7172756069788875 ) ) ;
#10500 = ORIENTED_EDGE ( 'NONE', *, *, #10141, .F. ) ;
#10501 = CARTESIAN_POINT ( 'NONE',  ( 9.371890508914830252E-13, 164.0000000000000000, -36.42135623730948168 ) ) ;
#10502 = DIRECTION ( 'NONE',  ( -1.000000000000000000, 0.000000000000000000, 0.000000000000000000 ) ) ;
#10503 = CARTESIAN_POINT ( 'NONE',  ( -951.7027691703365235, 118.7449601027238799, -141.4553492942759192 ) ) ;
#10504 = B_SPLINE_CURVE_WITH_KNOTS ( 'NONE', 3,
 ( #2036, #5925, #3949, #6787, #10561, #10619, #1235, #8711, #4990, #227, #7781, #11557, #8770, #4078, #6911, #10677, #2216, #10740, #3431, #466, #9124, #11855, #5348, #1352, #4191, #3312, #6170, #5119, #11677, #11740, #8882, #2391, #7093, #5172, #9878, #3195, #7968, #10857 ),
 .UNSPECIFIED., .F., .F.,
 ( 4, 2, 2, 2, 2, 2, 2, 2, 2, 2, 2, 2, 2, 2, 2, 2, 2, 2, 4 ),
 ( 1.387778780781445676E-17, 0.0009791294386043965323, 0.001958258877208779187, 0.002937388315813161625, 0.003916517754417544496, 0.004895647193021926934, 0.005874776631626309371, 0.006364341350928661920, 0.006853906070231015335, 0.007833035508835389099, 0.008812164947439762863, 0.009791294386044136627, 0.01077042382464851039, 0.01174955326325288589, 0.01272868270185725792, 0.01370781214046163342, 0.01468694157906600545, 0.01517650629836820447, 0.01566607101767040003 ),
 .UNSPECIFIED. ) ;
#10505 = AXIS2_PLACEMENT_3D ( 'NONE', #5765, #7631, #10529 ) ;
#10506 = SURFACE_SIDE_STYLE ('',( #7542 ) ) ;
#10507 = DIRECTION ( 'NONE',  ( -0.000000000000000000, 1.000000000000000000, -0.000000000000000000 ) ) ;
#10508 = ORIENTED_EDGE ( 'NONE', *, *, #8386, .F. ) ;
#10509 = DIRECTION ( 'NONE',  ( -1.000000000000000000, 0.000000000000000000, 0.000000000000000000 ) ) ;
#10510 = CARTESIAN_POINT ( 'NONE',  ( -1022.719357623492101, 104.5170332807324769, -149.7857175106632610 ) ) ;
#10511 = FACE_BOUND ( 'NONE', #4396, .T. ) ;
#10512 = ORIENTED_EDGE ( 'NONE', *, *, #7952, .F. ) ;
#10513 = CYLINDRICAL_SURFACE ( 'NONE', #2318, 7.500000000000007105 ) ;
#10514 = ORIENTED_EDGE ( 'NONE', *, *, #4342, .F. ) ;
#10515 = VECTOR ( 'NONE', #10958, 1000.000000000000000 ) ;
#10516 = ADVANCED_FACE ( 'NONE', ( #4773 ), #10513, .F. ) ;
#10517 = LINE ( 'NONE', #4664, #96 ) ;
#10518 = CARTESIAN_POINT ( 'NONE',  ( -819.3334343865132041, 76.46102376401721301, -105.4605772031392803 ) ) ;
#10519 = CARTESIAN_POINT ( 'NONE',  ( -1025.000791045970800, 67.42844482392692385, -149.7857175106636305 ) ) ;
#10520 = VERTEX_POINT ( 'NONE', #1193 ) ;
#10521 = CARTESIAN_POINT ( 'NONE',  ( -374.9804624535815947, 84.15814354082083071, -144.5772115629533232 ) ) ;
#10522 = CARTESIAN_POINT ( 'NONE',  ( 151.3258811035896656, 0.000000000000000000, -63.63263083939799003 ) ) ;
#10523 = EDGE_LOOP ( 'NONE', ( #619, #8956 ) ) ;
#10524 = ORIENTED_EDGE ( 'NONE', *, *, #10006, .T. ) ;
#10525 = ORIENTED_EDGE ( 'NONE', *, *, #9119, .F. ) ;
#10526 = FACE_OUTER_BOUND ( 'NONE', #5413, .T. ) ;
#10527 = AXIS2_PLACEMENT_3D ( 'NONE', #6775, #1046, #3071 ) ;
#10528 = CARTESIAN_POINT ( 'NONE',  ( -1024.641217300039216, 73.20632742167531148, -96.78565065507991960 ) ) ;
#10529 = DIRECTION ( 'NONE',  ( 4.236366511936864528E-16, -1.000000000000000000, -5.522905491341393153E-16 ) ) ;
#10530 = EDGE_CURVE ( 'NONE', #7375, #8861, #4092, .T. ) ;
#10531 = ADVANCED_FACE ( 'NONE', ( #6925 ), #11570, .T. ) ;
#10532 = ORIENTED_EDGE ( 'NONE', *, *, #1932, .T. ) ;
#10533 = DIRECTION ( 'NONE',  ( 0.000000000000000000, 0.000000000000000000, 1.000000000000000000 ) ) ;
#10534 = ORIENTED_EDGE ( 'NONE', *, *, #11249, .T. ) ;
#10535 = SHAPE_DEFINITION_REPRESENTATION ( #11481, #3601 ) ;
#10536 = ORIENTED_EDGE ( 'NONE', *, *, #342, .T. ) ;
#10537 = CARTESIAN_POINT ( 'NONE',  ( -901.8967518049364571, 57.00804855647901093, -118.7903414690679540 ) ) ;
#10538 = AXIS2_PLACEMENT_3D ( 'NONE', #9631, #7599, #10374 ) ;
#10539 = CARTESIAN_POINT ( 'NONE',  ( 9.371890508914830252E-13, -6.000000000000005329, -36.42135623730949590 ) ) ;
#10540 = AXIS2_PLACEMENT_3D ( 'NONE', #1369, #6127, #312 ) ;
#10541 = FACE_OUTER_BOUND ( 'NONE', #2355, .T. ) ;
#10542 = FACE_BOUND ( 'NONE', #5737, .T. ) ;
#10543 = FACE_BOUND ( 'NONE', #7998, .T. ) ;
#10544 = CARTESIAN_POINT ( 'NONE',  ( -19.99638601442813979, 178.7511098637216946, -125.0988180456752161 ) ) ;
#10545 = AXIS2_PLACEMENT_3D ( 'NONE', #3492, #5477, #11246 ) ;
#10546 = AXIS2_PLACEMENT_3D ( 'NONE', #11471, #6761, #1155 ) ;
#10547 = ORIENTED_EDGE ( 'NONE', *, *, #8137, .T. ) ;
#10548 = CIRCLE ( 'NONE', #7997, 81.99999999999998579 ) ;
#10549 = CARTESIAN_POINT ( 'NONE',  ( -374.7821307776476942, 76.37722585493098393, -154.0118767560747699 ) ) ;
#10550 = EDGE_CURVE ( 'NONE', #5774, #7370, #10725, .T. ) ;
#10551 = EDGE_CURVE ( 'NONE', #64, #10481, #5154, .T. ) ;
#10552 = SURFACE_STYLE_FILL_AREA ( #6777 ) ;
#10553 = EDGE_LOOP ( 'NONE', ( #1913, #9088 ) ) ;
#10554 = CARTESIAN_POINT ( 'NONE',  ( -952.4132309232843454, 101.5728619241205450, -96.78565065507918064 ) ) ;
#10555 = CARTESIAN_POINT ( 'NONE',  ( -3.161662739628749519E-15, 267.2792206135785591, -126.4213562373094959 ) ) ;
#10556 = EDGE_CURVE ( 'NONE', #1969, #6496, #1519, .T. ) ;
#10557 = AXIS2_PLACEMENT_3D ( 'NONE', #1658, #9133, #671 ) ;
#10558 = DIRECTION ( 'NONE',  ( -8.163404592832030268E-17, 1.000000000000000000, -0.000000000000000000 ) ) ;
#10559 = VERTEX_POINT ( 'NONE', #7829 ) ;
#10560 = CARTESIAN_POINT ( 'NONE',  ( -795.0000000000043201, 82.00000000000039790, -124.6807709998041105 ) ) ;
#10561 = CARTESIAN_POINT ( 'NONE',  ( -819.0811117622678239, 80.27710935352754973, -104.7528066153021626 ) ) ;
#10562 = DIRECTION ( 'NONE',  ( 0.000000000000000000, 1.000000000000000000, 0.000000000000000000 ) ) ;
#10563 = CARTESIAN_POINT ( 'NONE',  ( -1054.519145619990923, 111.4921997120091106, -136.2353035311978999 ) ) ;
#10564 = EDGE_CURVE ( 'NONE', #2268, #5951, #336, .T. ) ;
#10565 = TOROIDAL_SURFACE ( 'NONE', #12159, 19.00000000000000000, 1.000000000000000000 ) ;
#10566 = CARTESIAN_POINT ( 'NONE',  ( 13.32222501832767847, 180.2041921146325762, -184.1652315311843893 ) ) ;
#10567 = DIRECTION ( 'NONE',  ( 6.195440985631454085E-17, 0.000000000000000000, -1.000000000000000000 ) ) ;
#10568 = AXIS2_PLACEMENT_3D ( 'NONE', #3145, #8773, #1413 ) ;
#10569 = CARTESIAN_POINT ( 'NONE',  ( 7.500000000000000000, 0.000000000000000000, -6.599999999999998757 ) ) ;
#10570 = ORIENTED_EDGE ( 'NONE', *, *, #9179, .F. ) ;
#10571 = CARTESIAN_POINT ( 'NONE',  ( -992.5689194452182846, 110.2481211102048491, -146.0307792196443870 ) ) ;
#10572 = CARTESIAN_POINT ( 'NONE',  ( 35.00000000000000000, 81.99999999999998579, 190.3192290001959748 ) ) ;
#10573 = VERTEX_POINT ( 'NONE', #11604 ) ;
#10574 = AXIS2_PLACEMENT_3D ( 'NONE', #9865, #5159, #8073 ) ;
#10575 = ORIENTED_EDGE ( 'NONE', *, *, #11671, .F. ) ;
#10576 = CARTESIAN_POINT ( 'NONE',  ( -828.8285638327243987, 78.67432280806596623, -144.4023295390031194 ) ) ;
#10577 = CARTESIAN_POINT ( 'NONE',  ( -818.8285638327239440, 78.34163520102110567, -105.0153140909397393 ) ) ;
#10578 = CARTESIAN_POINT ( 'NONE',  ( 1.874378101782966050E-12, 163.9999999999999716, 61.07864376269052542 ) ) ;
#10579 = CARTESIAN_POINT ( 'NONE',  ( -1032.113539130925574, 67.34854938887519893, -152.5758913445294240 ) ) ;
#10580 = ORIENTED_EDGE ( 'NONE', *, *, #6319, .F. ) ;
#10581 = CARTESIAN_POINT ( 'NONE',  ( -374.4965189541518953, 90.54923481422481757, -153.1149316092644597 ) ) ;
#10582 = DIRECTION ( 'NONE',  ( 3.061276722312011504E-17, -1.000000000000000000, 0.000000000000000000 ) ) ;
#10583 = CARTESIAN_POINT ( 'NONE',  ( -374.9791051857908997, 79.82954463378038668, -104.7910636793791355 ) ) ;
#10584 =( LENGTH_UNIT ( ) NAMED_UNIT ( * ) SI_UNIT ( .MILLI., .METRE. ) );
#10585 = PRODUCT_DEFINITION_FORMATION_WITH_SPECIFIED_SOURCE ( 'ANY', '', #2006, .NOT_KNOWN. ) ;
#10586 = ORIENTED_EDGE ( 'NONE', *, *, #4727, .F. ) ;
#10587 = ORIENTED_EDGE ( 'NONE', *, *, #7462, .T. ) ;
#10588 = PRODUCT ( 'Mold for bends', 'Mold for bends', '', ( #3059 ) ) ;
#10589 = CYLINDRICAL_SURFACE ( 'NONE', #4863, 7.500000000000007105 ) ;
#10590 = CARTESIAN_POINT ( 'NONE',  ( -954.2862664537825594, 55.36536439393501041, -107.9061927053324439 ) ) ;
#10591 = CARTESIAN_POINT ( 'NONE',  ( 35.00000000000000000, 0.000000000000000000, 40.70327710424895429 ) ) ;
#10592 = CARTESIAN_POINT ( 'NONE',  ( -1028.454949082223038, 53.01113643315406421, -136.2353035311987810 ) ) ;
#10593 = EDGE_LOOP ( 'NONE', ( #6508, #4840, #5239, #6848 ) ) ;
#10594 = AXIS2_PLACEMENT_3D ( 'NONE', #2300, #11423, #40 ) ;
#10595 = CARTESIAN_POINT ( 'NONE',  ( -384.9968589487228883, 81.44061423874818217, -104.6863554354390118 ) ) ;
#10596 = ORIENTED_EDGE ( 'NONE', *, *, #3212, .F. ) ;
#10597 = CARTESIAN_POINT ( 'NONE',  ( -820.0628880458421008, 75.36885551798864924, -154.6770171190163126 ) ) ;
#10598 = ORIENTED_EDGE ( 'NONE', *, *, #2496, .T. ) ;
#10599 = EDGE_LOOP ( 'NONE', ( #9032, #545, #365, #12121 ) ) ;
#10600 = CARTESIAN_POINT ( 'NONE',  ( -1025.976186494711783, 52.68972726728017619, -122.7172756069792428 ) ) ;
#10601 = EDGE_CURVE ( 'NONE', #8983, #9452, #2716, .T. ) ;
#10602 = CARTESIAN_POINT ( 'NONE',  ( 0.09318607064170508769, 1.767053008316833651, -9.000000000000001776 ) ) ;
#10603 = DIRECTION ( 'NONE',  ( -8.163404592832030268E-17, 1.000000000000000000, -0.000000000000000000 ) ) ;
#10604 = CARTESIAN_POINT ( 'NONE',  ( 6.247927005943220505E-13, 0.000000000000000000, -58.92135623730948879 ) ) ;
#10605 = EDGE_CURVE ( 'NONE', #5042, #69, #11663, .T. ) ;
#10606 = CARTESIAN_POINT ( 'NONE',  ( -1011.418100375198719, 110.6663390795547599, -103.3307627799635782 ) ) ;
#10607 = DIRECTION ( 'NONE',  ( 1.000000000000000000, 0.000000000000000000, 0.000000000000000000 ) ) ;
#10608 = CARTESIAN_POINT ( 'NONE',  ( -19.99604380743649301, 177.7113426136561998, -125.1086484215899191 ) ) ;
#10609 = VERTEX_POINT ( 'NONE', #2617 ) ;
#10610 = DIRECTION ( 'NONE',  ( -0.000000000000000000, -1.000000000000000000, -0.000000000000000000 ) ) ;
#10611 = ORIENTED_EDGE ( 'NONE', *, *, #3726, .F. ) ;
#10612 = CARTESIAN_POINT ( 'NONE',  ( -1023.078931369429029, 98.73915068298381925, -96.78565065507928011 ) ) ;
#10613 = ORIENTED_EDGE ( 'NONE', *, *, #7952, .T. ) ;
#10614 = DIRECTION ( 'NONE',  ( 0.000000000000000000, 0.000000000000000000, 1.000000000000000000 ) ) ;
#10615 = EDGE_CURVE ( 'NONE', #5971, #1440, #3897, .T. ) ;
#10616 = CARTESIAN_POINT ( 'NONE',  ( -1060.756016675586807, 112.8516620848305934, -124.6807709998040821 ) ) ;
#10617 = ORIENTED_EDGE ( 'NONE', *, *, #389, .F. ) ;
#10618 = CARTESIAN_POINT ( 'NONE',  ( -852.8175266017511831, 121.6828083272127685, -124.6807709998041247 ) ) ;
#10619 = CARTESIAN_POINT ( 'NONE',  ( -819.3307005430665413, 80.88259174529672180, -104.7097040407755912 ) ) ;
#10620 = DIRECTION ( 'NONE',  ( 0.000000000000000000, -1.000000000000000000, 0.000000000000000000 ) ) ;
#10621 = CARTESIAN_POINT ( 'NONE',  ( -1046.095701327183860, 109.2451008237763546, -141.4553492942764308 ) ) ;
#10622 = CARTESIAN_POINT ( 'NONE',  ( -379.7973532621967934, 100.9195114153188797, -118.1876023976287087 ) ) ;
#10623 = CARTESIAN_POINT ( 'NONE',  ( 20.72709806565185531, 179.8688360349001414, -123.3353893985419774 ) ) ;
#10624 = VECTOR ( 'NONE', #8272, 1000.000000000000000 ) ;
#10625 = DIRECTION ( 'NONE',  ( 2.081668171172161734E-17, 4.930380657631307143E-31, -1.000000000000000000 ) ) ;
#10626 = DIRECTION ( 'NONE',  ( 2.081668171172161734E-17, 4.930380657631307143E-31, -1.000000000000000000 ) ) ;
#10627 =( NAMED_UNIT ( * ) SI_UNIT ( $, .STERADIAN. ) SOLID_ANGLE_UNIT ( ) );
#10628 = ORIENTED_EDGE ( 'NONE', *, *, #11356, .T. ) ;
#10629 = CARTESIAN_POINT ( 'NONE',  ( -828.8285638327247398, 78.67432280806576728, -154.5823979888776591 ) ) ;
#10630 = CARTESIAN_POINT ( 'NONE',  ( -1013.875822516560447, 120.2710389253235519, -124.6807709998039257 ) ) ;
#10631 = VECTOR ( 'NONE', #987, 1000.000000000000000 ) ;
#10632 = CYLINDRICAL_SURFACE ( 'NONE', #12084, 7.500000000000007105 ) ;
#10633 = FACE_BOUND ( 'NONE', #5399, .T. ) ;
#10634 = ORIENTED_EDGE ( 'NONE', *, *, #4942, .T. ) ;
#10635 = ADVANCED_FACE ( 'NONE', ( #9235 ), #5671, .T. ) ;
#10636 = VECTOR ( 'NONE', #9515, 1000.000000000000000 ) ;
#10637 = ORIENTED_EDGE ( 'NONE', *, *, #6665, .F. ) ;
#10638 = CARTESIAN_POINT ( 'NONE',  ( 19.91452063025001706, 178.8212236027263202, -122.8311025665217073 ) ) ;
#10639 = VECTOR ( 'NONE', #10702, 1000.000000000000000 ) ;
#10640 = CARTESIAN_POINT ( 'NONE',  ( -975.9242088207953429, 48.36955882740826240, -146.0307792196450407 ) ) ;
#10641 = CARTESIAN_POINT ( 'NONE',  ( -818.9567516184621354, 77.53771799247208207, -144.1773011583837558 ) ) ;
#10642 = EDGE_LOOP ( 'NONE', ( #7636, #3493, #3099, #7845 ) ) ;
#10643 = CARTESIAN_POINT ( 'NONE',  ( 0.3552109633437127156, -3.484997970589502447, -9.000000000000000000 ) ) ;
#10644 = AXIS2_PLACEMENT_3D ( 'NONE', #6431, #7301, #879 ) ;
#10645 = AXIS2_PLACEMENT_3D ( 'NONE', #5285, #9930, #5115 ) ;
#10646 = VERTEX_POINT ( 'NONE', #1573 ) ;
#10647 = ORIENTED_EDGE ( 'NONE', *, *, #10564, .F. ) ;
#10648 = LINE ( 'NONE', #3919, #6836 ) ;
#10649 = EDGE_CURVE ( 'NONE', #5163, #1219, #1927, .T. ) ;
#10650 = CARTESIAN_POINT ( 'NONE',  ( -976.0610374937461984, 42.74778062430068104, -107.9061927053324155 ) ) ;
#10651 = TOROIDAL_SURFACE ( 'NONE', #5313, 10.00000000000003730, 1.499999999999998002 ) ;
#10652 = CARTESIAN_POINT ( 'NONE',  ( -19.90963648991972690, 178.8974959161414233, -122.7794448225913584 ) ) ;
#10653 = EDGE_LOOP ( 'NONE', ( #2498, #11710, #1433, #4451 ) ) ;
#10654 = CARTESIAN_POINT ( 'NONE',  ( 28.00000000000000000, -6.000000000000000000, -27.99999999999999645 ) ) ;
#10655 = CARTESIAN_POINT ( 'NONE',  ( -383.8907576663274881, 90.90990570178517771, -106.7374497346880133 ) ) ;
#10656 = EDGE_LOOP ( 'NONE', ( #5200, #9698, #2954, #63 ) ) ;
#10657 = CARTESIAN_POINT ( 'NONE',  ( 0.000000000000000000, 0.000000000000000000, -126.4213562373094959 ) ) ;
#10658 = ORIENTED_EDGE ( 'NONE', *, *, #12070, .T. ) ;
#10659 = ITEM_DEFINED_TRANSFORMATION ( 'NONE', 'NONE', #305,  #11957 ) ;
#10660 = EDGE_LOOP ( 'NONE', ( #4702, #3772 ) ) ;
#10661 = CARTESIAN_POINT ( 'NONE',  ( -957.2086549536780922, 47.65337959301152893, -122.7172756069790012 ) ) ;
#10662 = LINE ( 'NONE', #9734, #1095 ) ;
#10663 = UNCERTAINTY_MEASURE_WITH_UNIT (LENGTH_MEASURE( 1.000000000000000082E-05 ), #230, 'distance_accuracy_value', 'NONE');
#10664 = CARTESIAN_POINT ( 'NONE',  ( -992.5689194452221500, 110.2481211102048491, -103.3307627799634218 ) ) ;
#10665 = CARTESIAN_POINT ( 'NONE',  ( -19.97123502809169793, 177.8744193083314826, -125.7706088136690852 ) ) ;
#10666 = EDGE_CURVE ( 'NONE', #11221, #7831, #4699, .T. ) ;
#10667 = ORIENTED_EDGE ( 'NONE', *, *, #3264, .T. ) ;
#10668 = DIRECTION ( 'NONE',  ( 0.000000000000000000, 0.000000000000000000, 1.000000000000000000 ) ) ;
#10669 = ORIENTED_EDGE ( 'NONE', *, *, #1692, .T. ) ;
#10670 = CARTESIAN_POINT ( 'NONE',  ( -1031.632959140997855, 88.47632675500361188, -95.06748246948018277 ) ) ;
#10671 = CARTESIAN_POINT ( 'NONE',  ( -951.4444194419925225, 124.5703232071644209, -130.5712005305403238 ) ) ;
#10672 = FACE_OUTER_BOUND ( 'NONE', #225, .T. ) ;
#10673 = CARTESIAN_POINT ( 'NONE',  ( 0.000000000000000000, 152.0000000000000000, -159.6807709998038547 ) ) ;
#10674 = CARTESIAN_POINT ( 'NONE',  ( -904.1919162299243453, 124.8346192645297918, -118.7903414690678119 ) ) ;
#10675 = ORIENTED_EDGE ( 'NONE', *, *, #10382, .F. ) ;
#10676 = DIRECTION ( 'NONE',  ( 0.000000000000000000, -1.000000000000000000, -7.930164461608263644E-17 ) ) ;
#10677 = CARTESIAN_POINT ( 'NONE',  ( -822.5306970061909624, 83.50573423571496789, -104.7374748144103336 ) ) ;
#10678 = CARTESIAN_POINT ( 'NONE',  ( 0.000000000000000000, -492.9999999999998863, 0.000000000000000000 ) ) ;
#10679 = ADVANCED_FACE ( 'NONE', ( #7198 ), #12018, .F. ) ;
#10680 = CARTESIAN_POINT ( 'NONE',  ( 21.06824446939009121, 179.1652731564143721, -126.0114239279031807 ) ) ;
#10681 = CARTESIAN_POINT ( 'NONE',  ( -35.00000000000000000, 12.00000000000000000, 40.70327710424895429 ) ) ;
#10682 = EDGE_CURVE ( 'NONE', #2378, #4910, #8828, .T. ) ;
#10683 = VERTEX_POINT ( 'NONE', #4359 ) ;
#10684 = DIRECTION ( 'NONE',  ( 0.000000000000000000, 1.000000000000000000, 0.000000000000000000 ) ) ;
#10685 = CARTESIAN_POINT ( 'NONE',  ( -305.0000000000000568, 81.99999999999995737, -89.68077099980384048 ) ) ;
#10686 = EDGE_CURVE ( 'NONE', #8172, #5876, #11227, .T. ) ;
#10687 = PRODUCT_DEFINITION_SHAPE ( 'NONE', 'NONE',  #12244 ) ;
#10688 = CYLINDRICAL_SURFACE ( 'NONE', #11687, 7.500000000000007994 ) ;
#10689 = CARTESIAN_POINT ( 'NONE',  ( -903.8503739047791896, 115.2915043052427251, -146.0307792196441881 ) ) ;
#10690 = CARTESIAN_POINT ( 'NONE',  ( -154.5043356068770493, 0.000000000000000000, -102.0666613060160302 ) ) ;
#10691 = VECTOR ( 'NONE', #5057, 1000.000000000000000 ) ;
#10692 = CARTESIAN_POINT ( 'NONE',  ( 126.4213562373094959, 12.00000000000000000, -6.938893903907228378E-15 ) ) ;
#10693 = CARTESIAN_POINT ( 'NONE',  ( 6.899999999999999467, 8.999999999999998224, 0.000000000000000000 ) ) ;
#10694 = ORIENTED_EDGE ( 'NONE', *, *, #2021, .T. ) ;
#10695 = CARTESIAN_POINT ( 'NONE',  ( -1060.756016675586807, 112.8516620848305934, -124.6807709998040821 ) ) ;
#10696 = CARTESIAN_POINT ( 'NONE',  ( -927.8303129675907712, 79.95948428978974221, -152.5758913445291682 ) ) ;
#10697 = CARTESIAN_POINT ( 'NONE',  ( -820.0477536417098463, 75.38653579115424463, -143.5572547269229062 ) ) ;
#10698 = CIRCLE ( 'NONE', #1044, 7.500000000000007105 ) ;
#10699 = CARTESIAN_POINT ( 'NONE',  ( -374.5266264499630324, 90.13403016665176892, -153.2070368496501658 ) ) ;
#10700 = CARTESIAN_POINT ( 'NONE',  ( -126.4213562373094959, -492.9999999999998863, -7.499999999999990230 ) ) ;
#10701 = ADVANCED_FACE ( 'NONE', ( #4419 ), #9813, .F. ) ;
#10702 = DIRECTION ( 'NONE',  ( -0.000000000000000000, -0.000000000000000000, -1.000000000000000000 ) ) ;
#10704 = EDGE_CURVE ( 'NONE', #11382, #7316, #8129, .T. ) ;
#10703 = DIRECTION ( 'NONE',  ( 0.000000000000000000, 0.000000000000000000, -1.000000000000000000 ) ) ;
#10705 = EDGE_LOOP ( 'NONE', ( #11680, #8078, #7488, #3115, #7736, #5302 ) ) ;
#10706 = CARTESIAN_POINT ( 'NONE',  ( -1014.107508992743988, 52.59077491224116585, -130.5712005305404944 ) ) ;
#10707 = CIRCLE ( 'NONE', #2414, 20.00000000000017053 ) ;
#10708 = ORIENTED_EDGE ( 'NONE', *, *, #5752, .F. ) ;
#10709 = CARTESIAN_POINT ( 'NONE',  ( -1065.000000000004093, 52.00000000000021316, -122.7172756069792854 ) ) ;
#10710 = DIRECTION ( 'NONE',  ( -0.000000000000000000, 1.000000000000000000, -1.224646799147353207E-16 ) ) ;
#10711 = CARTESIAN_POINT ( 'NONE',  ( -277.5000000000000000, -9.213203435596478030, -126.4213562373076059 ) ) ;
#10712 = PLANE ( 'NONE',  #10944 ) ;
#10713 = APPLICATION_CONTEXT ( 'automotive_design' ) ;
#10714 = DIRECTION ( 'NONE',  ( 0.000000000000000000, -1.000000000000000000, 0.000000000000000000 ) ) ;
#10715 = DIRECTION ( 'NONE',  ( 1.000000000000000000, 1.186840563529527301E-16, 0.000000000000000000 ) ) ;
#10716 = CARTESIAN_POINT ( 'NONE',  ( -828.5739595068184826, 77.06538570633833274, -154.6543796050835624 ) ) ;
#10717 = VERTEX_POINT ( 'NONE', #8196 ) ;
#10718 = CONTEXT_DEPENDENT_SHAPE_REPRESENTATION ( #6758, #3094 ) ;
#10719 = ORIENTED_EDGE ( 'NONE', *, *, #10735, .F. ) ;
#10720 = CARTESIAN_POINT ( 'NONE',  ( -1014.004070199759440, 54.58258344709550869, -113.1262384684095537 ) ) ;
#10721 = DIRECTION ( 'NONE',  ( 2.040851148208007875E-17, -1.000000000000000000, -0.000000000000000000 ) ) ;
#10722 = DIRECTION ( 'NONE',  ( 1.224646799147349509E-16, 0.000000000000000000, -1.000000000000000000 ) ) ;
#10723 = AXIS2_PLACEMENT_3D ( 'NONE', #9957, #10945, #5134 ) ;
#10724 = CARTESIAN_POINT ( 'NONE',  ( -1046.676250823070177, 92.10743237175765330, -96.78565065507946485 ) ) ;
#10725 = LINE ( 'NONE', #10787, #3486 ) ;
#10726 = DIRECTION ( 'NONE',  ( -1.000000000000000000, -0.000000000000000000, -0.000000000000000000 ) ) ;
#10727 = EDGE_LOOP ( 'NONE', ( #10924, #563, #5996, #5336 ) ) ;
#10728 = CARTESIAN_POINT ( 'NONE',  ( 35.00000000000000000, 0.000000000000000000, 190.3192290001959464 ) ) ;
#10729 = AXIS2_PLACEMENT_3D ( 'NONE', #12211, #5651, #9423 ) ;
#10730 = VERTEX_POINT ( 'NONE', #11959 ) ;
#10731 = CARTESIAN_POINT ( 'NONE',  ( -1065.000000000005912, 82.00000000000039790, -94.48732055948609343 ) ) ;
#10732 = DIRECTION ( 'NONE',  ( 0.000000000000000000, 0.000000000000000000, 1.000000000000000000 ) ) ;
#10733 = CARTESIAN_POINT ( 'NONE',  ( -974.1288507787421622, 124.2142274477007078, -126.6442663926288787 ) ) ;
#10734 = CYLINDRICAL_SURFACE ( 'NONE', #6492, 7.500000000000007105 ) ;
#10735 = EDGE_CURVE ( 'NONE', #2073, #10209, #4493, .T. ) ;
#10736 = CIRCLE ( 'NONE', #8577, 7.500000000000007105 ) ;
#10737 = VECTOR ( 'NONE', #9638, 1000.000000000000000 ) ;
#10738 = CARTESIAN_POINT ( 'NONE',  ( -1021.777026427247165, 118.8177985574657924, -118.7903414690675561 ) ) ;
#10739 = CARTESIAN_POINT ( 'NONE',  ( 151.3258811035896656, 12.00000000000000000, -63.63263083939799003 ) ) ;
#10740 = CARTESIAN_POINT ( 'NONE',  ( -823.1752771847263830, 83.64233931405162537, -104.7482132693508419 ) ) ;
#10741 = DIRECTION ( 'NONE',  ( 1.000000000000000000, 1.486905836551548832E-16, -0.000000000000000000 ) ) ;
#10742 = CARTESIAN_POINT ( 'NONE',  ( -373.0282128842003431, 99.74530980265677726, -115.3648426268730276 ) ) ;
#10743 = SURFACE_SIDE_STYLE ('',( #5051 ) ) ;
#10744 = DIRECTION ( 'NONE',  ( 1.000000000000000000, 3.061276722312011504E-17, 0.000000000000000000 ) ) ;
#10745 = EDGE_LOOP ( 'NONE', ( #9584, #8682, #7043, #8805 ) ) ;
#10746 = DIRECTION ( 'NONE',  ( -1.000000000000000000, 0.000000000000000000, 0.000000000000000000 ) ) ;
#10747 = DIRECTION ( 'NONE',  ( 0.000000000000000000, 0.000000000000000000, 1.000000000000000000 ) ) ;
#10748 = CARTESIAN_POINT ( 'NONE',  ( -926.5138833012647410, 125.7648744980332225, -124.6807709998040394 ) ) ;
#10749 = VECTOR ( 'NONE', #53, 1000.000000000000000 ) ;
#10750 = DIRECTION ( 'NONE',  ( 0.000000000000000000, 0.000000000000000000, 1.000000000000000000 ) ) ;
#10751 = EDGE_CURVE ( 'NONE', #8782, #4959, #3694, .T. ) ;
#10752 = DIRECTION ( 'NONE',  ( -1.000000000000000000, 0.000000000000000000, 0.000000000000000000 ) ) ;
#10753 = ADVANCED_FACE ( 'NONE', ( #6822 ), #1022, .F. ) ;
#10754 = EDGE_LOOP ( 'NONE', ( #9095, #10658, #11628, #11743 ) ) ;
#10755 = EDGE_LOOP ( 'NONE', ( #10587, #1598, #3325 ) ) ;
#10756 = CIRCLE ( 'NONE', #8005, 7.500000000000007105 ) ;
#10757 = CARTESIAN_POINT ( 'NONE',  ( -380.1407962618786200, 63.69369713673138023, -132.7567463350160892 ) ) ;
#10758 = CARTESIAN_POINT ( 'NONE',  ( -1047.151245865163673, 77.61790247226322492, -154.8742214401233070 ) ) ;
#10759 = CARTESIAN_POINT ( 'NONE',  ( -374.1268486318114128, 93.09154424955353591, -151.9171935354461596 ) ) ;
#10760 = CARTESIAN_POINT ( 'NONE',  ( 1.561981751485805177E-12, 152.0000000000000000, 23.57864376269051832 ) ) ;
#10761 = CARTESIAN_POINT ( 'NONE',  ( -373.1046688609678768, 64.56459520230322369, -114.7895357036745025 ) ) ;
#10762 = FACE_OUTER_BOUND ( 'NONE', #6813, .T. ) ;
#10763 = SURFACE_STYLE_FILL_AREA ( #9535 ) ;
#10764 = ORIENTED_EDGE ( 'NONE', *, *, #7457, .F. ) ;
#10765 = CARTESIAN_POINT ( 'NONE',  ( -956.9243412622475944, 54.10650223846812423, -141.4553492942761181 ) ) ;
#10766 = CIRCLE ( 'NONE', #10568, 20.00000000000000000 ) ;
#10767 = ORIENTED_EDGE ( 'NONE', *, *, #10837, .T. ) ;
#10768 = EDGE_CURVE ( 'NONE', #10331, #11346, #10218, .T. ) ;
#10769 = ADVANCED_FACE ( 'NONE', ( #8971 ), #8246, .F. ) ;
#10770 = CARTESIAN_POINT ( 'NONE',  ( -957.0819499390169085, 50.45265437475560333, -113.1262384684095537 ) ) ;
#10771 = DIRECTION ( 'NONE',  ( 1.000000000000000000, 0.000000000000000000, 0.000000000000000000 ) ) ;
#10772 = ORIENTED_EDGE ( 'NONE', *, *, #10976, .T. ) ;
#10773 = DIRECTION ( 'NONE',  ( -8.163404592832030268E-17, 1.000000000000000000, -0.000000000000000000 ) ) ;
#10774 =( GEOMETRIC_REPRESENTATION_CONTEXT ( 3 ) GLOBAL_UNCERTAINTY_ASSIGNED_CONTEXT ( ( #4693 ) ) GLOBAL_UNIT_ASSIGNED_CONTEXT ( ( #8076, #5864, #10627 ) ) REPRESENTATION_CONTEXT ( 'NONE', 'WORKASPACE' ) );
#10775 = LINE ( 'NONE', #11771, #10515 ) ;
#10776 = ORIENTED_EDGE ( 'NONE', *, *, #6901, .F. ) ;
#10777 = CARTESIAN_POINT ( 'NONE',  ( -828.8285638327248535, 78.34854159839228771, -154.6011532199805174 ) ) ;
#10778 = ORIENTED_EDGE ( 'NONE', *, *, #1316, .T. ) ;
#10779 = EDGE_CURVE ( 'NONE', #11480, #11382, #4539, .T. ) ;
#10780 = ORIENTED_EDGE ( 'NONE', *, *, #9158, .T. ) ;
#10781 = CARTESIAN_POINT ( 'NONE',  ( -1017.133222628208614, 54.07990892584129483, -118.7903414690683519 ) ) ;
#10782 = CARTESIAN_POINT ( 'NONE',  ( 1.387778780781445676E-14, -6.000000000000000000, 126.4213562373094959 ) ) ;
#10783 = AXIS2_PLACEMENT_3D ( 'NONE', #4969, #2081, #6706 ) ;
#10784 = DIRECTION ( 'NONE',  ( 0.000000000000000000, 1.000000000000000000, 0.000000000000000000 ) ) ;
#10785 = ADVANCED_FACE ( 'NONE', ( #5322, #4404, #5813, #2052, #3724, #2800, #7678, #6570, #1011, #10335, #1935 ), #5640, .F. ) ;
#10786 = CARTESIAN_POINT ( 'NONE',  ( -1046.261572611724432, 104.4651992465225447, -103.3307627799636208 ) ) ;
#10787 = CARTESIAN_POINT ( 'NONE',  ( -82.49999999999997158, -9.213203435596451385, -126.4213562373088564 ) ) ;
#10788 = CARTESIAN_POINT ( 'NONE',  ( -19.99537293950516670, 177.7157818389469242, -125.1249387510345912 ) ) ;
#10789 = ORIENTED_EDGE ( 'NONE', *, *, #6134, .T. ) ;
#10790 = DIRECTION ( 'NONE',  ( 0.000000000000000000, 1.000000000000000000, 0.000000000000000000 ) ) ;
#10791 = VERTEX_POINT ( 'NONE', #11325 ) ;
#10792 = CARTESIAN_POINT ( 'NONE',  ( -22.49999999999999289, 152.0000000000000000, -126.4213562373092685 ) ) ;
#10793 = CARTESIAN_POINT ( 'NONE',  ( -1011.935294340108044, 99.50314415908297860, -96.78565065507922327 ) ) ;
#10794 = VECTOR ( 'NONE', #5373, 1000.000000000000000 ) ;
#10795 = DIRECTION ( 'NONE',  ( -8.163404592832031500E-17, 1.000000000000000000, 0.000000000000000000 ) ) ;
#10796 = CARTESIAN_POINT ( 'NONE',  ( -1045.864486809339724, 115.5688325305733741, -124.6807709998043663 ) ) ;
#10797 = CARTESIAN_POINT ( 'NONE',  ( 19.83679575339899159, 180.6775276936280079, -127.2308936265927315 ) ) ;
#10798 = CARTESIAN_POINT ( 'NONE',  ( 19.99669161722127697, 177.7723063827659473, -124.2664439125946103 ) ) ;
#10799 = DIRECTION ( 'NONE',  ( -1.186840563529527301E-16, 1.000000000000000000, -0.000000000000000000 ) ) ;
#10800 = CARTESIAN_POINT ( 'NONE',  ( -818.8285638327206470, 78.67432280806529832, -144.4023295390026931 ) ) ;
#10801 = FACE_BOUND ( 'NONE', #8520, .T. ) ;
#10802 = DIRECTION ( 'NONE',  ( 0.000000000000000000, 0.000000000000000000, 1.000000000000000000 ) ) ;
#10803 = AXIS2_PLACEMENT_3D ( 'NONE', #7233, #318, #549 ) ;
#10804 = CARTESIAN_POINT ( 'NONE',  ( -818.9960188511360002, 79.96793249489842026, -94.81477973375639579 ) ) ;
#10805 = CARTESIAN_POINT ( 'NONE',  ( -305.0000000000000568, 24.00000000000000711, -89.68077099980384048 ) ) ;
#10806 = ORIENTED_EDGE ( 'NONE', *, *, #4322, .T. ) ;
#10807 = CARTESIAN_POINT ( 'NONE',  ( -270.0000000000000000, -9.213203435596478030, -126.4213562373076059 ) ) ;
#10808 = DIRECTION ( 'NONE',  ( 0.000000000000000000, -1.000000000000000000, -7.930164461608263644E-17 ) ) ;
#10809 = CARTESIAN_POINT ( 'NONE',  ( -819.8285638327247398, 78.67432280806536937, -158.6807709998041673 ) ) ;
#10810 = CARTESIAN_POINT ( 'NONE',  ( -375.0000000000001705, 81.27848041085138675, -94.68077099980376943 ) ) ;
#10811 = VECTOR ( 'NONE', #4156, 1000.000000000000000 ) ;
#10812 = CARTESIAN_POINT ( 'NONE',  ( -6.360897667028196044E-14, -494.9999999999998863, -141.4213562373094817 ) ) ;
#10813 = ORIENTED_EDGE ( 'NONE', *, *, #11458, .F. ) ;
#10814 = VECTOR ( 'NONE', #594, 1000.000000000000000 ) ;
#10815 = LINE ( 'NONE', #1487, #5802 ) ;
#10816 = AXIS2_PLACEMENT_3D ( 'NONE', #7534, #7594, #4577 ) ;
#10817 = EDGE_CURVE ( 'NONE', #1708, #3156, #7443, .T. ) ;
#10818 = DIRECTION ( 'NONE',  ( 3.061276722312011504E-17, -1.000000000000000000, 0.000000000000000000 ) ) ;
#10819 = CARTESIAN_POINT ( 'NONE',  ( -126.4213562373094959, -494.9999999999998863, -7.499999999999990230 ) ) ;
#10820 = CARTESIAN_POINT ( 'NONE',  ( -7.500000000000007105, 152.0000000000000000, -126.4213562373094959 ) ) ;
#10821 = EDGE_CURVE ( 'NONE', #11612, #7375, #12198, .T. ) ;
#10822 = FACE_OUTER_BOUND ( 'NONE', #10001, .T. ) ;
#10823 = ORIENTED_EDGE ( 'NONE', *, *, #11154, .F. ) ;
#10824 = CARTESIAN_POINT ( 'NONE',  ( -817.4144546772251942, 30.82543593413060279, -136.2353035311987242 ) ) ;
#10825 = CIRCLE ( 'NONE', #7070, 1.499999999999998224 ) ;
#10826 = AXIS2_PLACEMENT_3D ( 'NONE', #3625, #1789, #5554 ) ;
#10827 = EDGE_LOOP ( 'NONE', ( #7979, #9904 ) ) ;
#10828 = ADVANCED_FACE ( 'NONE', ( #9529 ), #7733, .T. ) ;
#10829 = CARTESIAN_POINT ( 'NONE',  ( 20.00073208655986079, 178.6939288504570129, -124.5619098010894277 ) ) ;
#10830 = CARTESIAN_POINT ( 'NONE',  ( -795.0000000000050022, 56.89504896194521422, -107.9061927053325860 ) ) ;
#10831 = DIRECTION ( 'NONE',  ( 0.000000000000000000, 0.000000000000000000, 1.000000000000000000 ) ) ;
#10832 = CIRCLE ( 'NONE', #571, 7.500000000000007105 ) ;
#10833 = DIRECTION ( 'NONE',  ( 0.000000000000000000, -1.000000000000000000, 0.000000000000000000 ) ) ;
#10834 = CLOSED_SHELL ( 'NONE', ( #6257, #2782, #4502, #5250, #9845, #11303, #8573, #1527, #5995, #6166, #4413, #11215, #10531, #11582, #4804, #9881, #3645, #10402, #9265, #3875, #11321, #8055, #6182, #1610, #11688, #11881, #8663, #12041, #10701 ) ) ;
#10835 = EDGE_LOOP ( 'NONE', ( #10276, #576, #327, #4646, #3031 ) ) ;
#10836 = VERTEX_POINT ( 'NONE', #10578 ) ;
#10837 = EDGE_CURVE ( 'NONE', #4751, #2076, #3048, .T. ) ;
#10838 = FACE_OUTER_BOUND ( 'NONE', #5087, .T. ) ;
#10839 = AXIS2_PLACEMENT_3D ( 'NONE', #10264, #2845, #1738 ) ;
#10840 = TOROIDAL_SURFACE ( 'NONE', #1972, 4.000000000000045297, 1.000000000000000000 ) ;
#10841 = CARTESIAN_POINT ( 'NONE',  ( -157.5000000000000000, 152.0000000000000000, -126.4213562373084301 ) ) ;
#10842 = CARTESIAN_POINT ( 'NONE',  ( -1065.000000000005230, 87.89043812168627312, -95.06748246948058068 ) ) ;
#10843 = CARTESIAN_POINT ( 'NONE',  ( -19.99906152404484061, 177.7018673789226568, -124.9038452892194329 ) ) ;
#10844 = VERTEX_POINT ( 'NONE', #11507 ) ;
#10845 = CARTESIAN_POINT ( 'NONE',  ( -374.8742850566777634, 86.27977464002199781, -95.06579166030898875 ) ) ;
#10846 = EDGE_LOOP ( 'NONE', ( #12138, #6098 ) ) ;
#10847 = DIRECTION ( 'NONE',  ( 0.000000000000000000, 1.000000000000000000, 0.000000000000000000 ) ) ;
#10848 = CARTESIAN_POINT ( 'NONE',  ( 6.899999999999999467, 0.000000000000000000, 0.000000000000000000 ) ) ;
#10849 = ORIENTED_EDGE ( 'NONE', *, *, #6928, .F. ) ;
#10850 = DIRECTION ( 'NONE',  ( -1.000000000000000000, 0.000000000000000000, 0.000000000000000000 ) ) ;
#10851 = CARTESIAN_POINT ( 'NONE',  ( -1062.096538105501168, 73.81465972843167833, -95.06748246948046699 ) ) ;
#10852 = EDGE_CURVE ( 'NONE', #5780, #2194, #10548, .T. ) ;
#10853 = CARTESIAN_POINT ( 'NONE',  ( 19.91813571189143417, 181.6502384987539926, -122.8703185013854409 ) ) ;
#10854 = CARTESIAN_POINT ( 'NONE',  ( -795.0000000000040927, 111.6133447792292088, -130.5712005305403522 ) ) ;
#10855 = CARTESIAN_POINT ( 'NONE',  ( 19.89204199682034258, 179.2535526226286606, -122.6034008110078304 ) ) ;
#10856 = DIRECTION ( 'NONE',  ( 0.000000000000000000, 1.000000000000000000, 0.000000000000000000 ) ) ;
#10857 = CARTESIAN_POINT ( 'NONE',  ( -828.8285638327206470, 78.67432280806529832, -104.9592124606049879 ) ) ;
#10858 = CARTESIAN_POINT ( 'NONE',  ( -379.2722913866882664, 62.18251865808234413, -121.9290846803070849 ) ) ;
#10859 = CARTESIAN_POINT ( 'NONE',  ( -820.0616184920847900, 81.97828950705842033, -95.00646471220841249 ) ) ;
#10860 = VERTEX_POINT ( 'NONE', #319 ) ;
#10861 = DIRECTION ( 'NONE',  ( 0.000000000000000000, 0.000000000000000000, 1.000000000000000000 ) ) ;
#10862 = CARTESIAN_POINT ( 'NONE',  ( -795.0000000000046612, 112.0000000000007532, -122.7172756069791717 ) ) ;
#10863 = CARTESIAN_POINT ( 'NONE',  ( 0.000000000000000000, 0.000000000000000000, 0.000000000000000000 ) ) ;
#10864 = DIRECTION ( 'NONE',  ( -8.163404592832030268E-17, 1.000000000000000000, -0.000000000000000000 ) ) ;
#10865 = DIRECTION ( 'NONE',  ( 0.000000000000000000, 1.000000000000000000, 0.000000000000000000 ) ) ;
#10866 = ORIENTED_EDGE ( 'NONE', *, *, #10896, .T. ) ;
#10867 = VERTEX_POINT ( 'NONE', #4221 ) ;
#10868 = CARTESIAN_POINT ( 'NONE',  ( 19.87433925290471848, 179.8947790015472208, -122.4423054685512113 ) ) ;
#10869 = AXIS2_PLACEMENT_3D ( 'NONE', #1280, #1392, #4173 ) ;
#10870 = CARTESIAN_POINT ( 'NONE',  ( -384.2568156453588131, 74.72561187594924093, -143.3202744651779312 ) ) ;
#10871 = CARTESIAN_POINT ( 'NONE',  ( -975.3893330992545998, 71.12659035875127245, -154.2940595301280950 ) ) ;
#10872 = CARTESIAN_POINT ( 'NONE',  ( -826.9024563477421452, 74.71743289348884787, -143.3087845970618162 ) ) ;
#10873 = ORIENTED_EDGE ( 'NONE', *, *, #8952, .T. ) ;
#10874 = CARTESIAN_POINT ( 'NONE',  ( -370.5975445210319776, 106.4368310733506746, -135.7352130142525937 ) ) ;
#10875 = CARTESIAN_POINT ( 'NONE',  ( 0.3552109633508168662, -3.484997970623485930, 8.999999999999998224 ) ) ;
#10876 = CARTESIAN_POINT ( 'NONE',  ( -826.0494213903788250, 74.18265558624132439, -94.69403889809616715 ) ) ;
#10877 = SURFACE_STYLE_FILL_AREA ( #623 ) ;
#10878 = ORIENTED_EDGE ( 'NONE', *, *, #5649, .F. ) ;
#10879 = CARTESIAN_POINT ( 'NONE',  ( -853.9759289228051102, 31.63339360934212152, -141.4553492942759192 ) ) ;
#10880 = VERTEX_POINT ( 'NONE', #4107 ) ;
#10881 = ADVANCED_FACE ( 'NONE', ( #6942 ), #10712, .T. ) ;
#10882 = ORIENTED_EDGE ( 'NONE', *, *, #3822, .F. ) ;
#10883 = CARTESIAN_POINT ( 'NONE',  ( 87.04832655144112152, 12.00000000000000000, -217.9289243767383368 ) ) ;
#10884 = CARTESIAN_POINT ( 'NONE',  ( 19.98584444751550393, 177.8987813746903441, -123.9137298384522836 ) ) ;
#10885 = AXIS2_PLACEMENT_3D ( 'NONE', #8779, #236, #6120 ) ;
#10886 = CARTESIAN_POINT ( 'NONE',  ( -19.87519864879852349, 178.8871479037923393, -126.9115732480538838 ) ) ;
#10887 = DIRECTION ( 'NONE',  ( -0.000000000000000000, 1.000000000000000000, -0.000000000000000000 ) ) ;
#10888 = CARTESIAN_POINT ( 'NONE',  ( -828.1603582063153226, 81.17680912107698532, -94.97408237440919265 ) ) ;
#10889 = DIRECTION ( 'NONE',  ( -8.163404592832030268E-17, 1.000000000000000000, -0.000000000000000000 ) ) ;
#10890 = ORIENTED_EDGE ( 'NONE', *, *, #2427, .F. ) ;
#10891 = DIRECTION ( 'NONE',  ( 0.000000000000000000, 0.000000000000000000, 1.000000000000000000 ) ) ;
#10892 = CIRCLE ( 'NONE', #5573, 7.500000000000007105 ) ;
#10893 = ORIENTED_EDGE ( 'NONE', *, *, #8508, .T. ) ;
#10894 = AXIS2_PLACEMENT_3D ( 'NONE', #7287, #2579, #6351 ) ;
#10895 = FACE_OUTER_BOUND ( 'NONE', #260, .T. ) ;
#10896 = EDGE_CURVE ( 'NONE', #3571, #10683, #6017, .T. ) ;
#10897 = CARTESIAN_POINT ( 'NONE',  ( 0.000000000000000000, 7.794228634059941818, -4.500000000000007994 ) ) ;
#10898 = ADVANCED_FACE ( 'NONE', ( #1323 ), #770, .F. ) ;
#10899 = CARTESIAN_POINT ( 'NONE',  ( -903.0443340174317655, 90.92133391050421665, -94.48732055948569553 ) ) ;
#10900 = CARTESIAN_POINT ( 'NONE',  ( -172.5000000000000000, -9.213203435596478030, -126.4213562373082453 ) ) ;
#10901 = CARTESIAN_POINT ( 'NONE',  ( -375.0000000000000568, 82.00000000000093792, -94.68077099980381206 ) ) ;
#10902 = VERTEX_POINT ( 'NONE', #9237 ) ;
#10903 = FACE_OUTER_BOUND ( 'NONE', #7900, .T. ) ;
#10904 = DIRECTION ( 'NONE',  ( 0.000000000000000000, 0.000000000000000000, 1.000000000000000000 ) ) ;
#10905 = ORIENTED_EDGE ( 'NONE', *, *, #948, .T. ) ;
#10906 = CARTESIAN_POINT ( 'NONE',  ( -44.00000000000000000, 24.00000000000001776, -126.4213562373094959 ) ) ;
#10907 = EDGE_CURVE ( 'NONE', #5463, #11012, #778, .T. ) ;
#10908 = B_SPLINE_CURVE_WITH_KNOTS ( 'NONE', 3,
 ( #804, #9262, #12113, #3624, #7412, #6483, #1853, #2841, #3761, #9450, #10437, #1978, #4415, #8189, #8913, #6143 ),
 .UNSPECIFIED., .F., .F.,
 ( 4, 2, 2, 2, 2, 2, 2, 4 ),
 ( 0.0009136864633593878935, 0.001421019263031339909, 0.001928352062703291925, 0.002435684862375243724, 0.002943017662047195740, 0.003450350461719148623, 0.003957683261391099772, 0.004972348860735044569 ),
 .UNSPECIFIED. ) ;
#10909 = DIRECTION ( 'NONE',  ( 0.000000000000000000, 1.000000000000000000, 0.000000000000000000 ) ) ;
#10910 = ORIENTED_EDGE ( 'NONE', *, *, #1319, .F. ) ;
#10911 = LINE ( 'NONE', #9988, #2122 ) ;
#10912 = CARTESIAN_POINT ( 'NONE',  ( -1056.430032577878137, 71.19035303699463668, -95.06748246948046699 ) ) ;
#10913 = AXIS2_PLACEMENT_3D ( 'NONE', #663, #12038, #2573 ) ;
#10914 = CARTESIAN_POINT ( 'NONE',  ( -142.5000000000000000, 12.00000000000001421, -126.4213562373084301 ) ) ;
#10915 = CARTESIAN_POINT ( 'NONE',  ( -21.06624625262745099, 181.3699762841097538, -125.8703140475546149 ) ) ;
#10916 = DIRECTION ( 'NONE',  ( 1.000000000000000000, 0.000000000000000000, 0.000000000000000000 ) ) ;
#10917 = CARTESIAN_POINT ( 'NONE',  ( -1013.901471336336158, 119.8325901201402814, -118.7903414690677835 ) ) ;
#10918 = CARTESIAN_POINT ( 'NONE',  ( 1.561981751485805177E-12, 0.000000000000000000, 23.57864376269050410 ) ) ;
#10919 = CARTESIAN_POINT ( 'NONE',  ( -19.95147628160284370, 182.1113810128487387, -123.2819571381896822 ) ) ;
#10920 = TOROIDAL_SURFACE ( 'NONE', #5600, 6.500000000000005329, 1.000000000000000000 ) ;
#10921 = EDGE_CURVE ( 'NONE', #8735, #11690, #8960, .T. ) ;
#10922 = FACE_BOUND ( 'NONE', #626, .T. ) ;
#10923 = DIRECTION ( 'NONE',  ( 0.000000000000000000, 0.000000000000000000, -1.000000000000000000 ) ) ;
#10924 = ORIENTED_EDGE ( 'NONE', *, *, #6406, .T. ) ;
#10925 = DIRECTION ( 'NONE',  ( 0.000000000000000000, 0.000000000000000000, 1.000000000000000000 ) ) ;
#10926 = CARTESIAN_POINT ( 'NONE',  ( -991.5701548301636876, 122.8678427087060214, -124.6807709998040536 ) ) ;
#10927 = EDGE_CURVE ( 'NONE', #20, #12185, #5017, .T. ) ;
#10928 = EDGE_CURVE ( 'NONE', #8918, #1810, #7871, .T. ) ;
#10929 = DIRECTION ( 'NONE',  ( 0.7071067811865473507, 0.000000000000000000, -0.7071067811865477948 ) ) ;
#10930 = DIRECTION ( 'NONE',  ( -1.000000000000000000, 0.000000000000000000, 0.000000000000000000 ) ) ;
#10931 = FACE_OUTER_BOUND ( 'NONE', #8499, .T. ) ;
#10932 = VECTOR ( 'NONE', #3639, 1000.000000000000000 ) ;
#10933 = CARTESIAN_POINT ( 'NONE',  ( -6.360897667028196044E-14, -6.000000000000000000, -141.4213562373094817 ) ) ;
#10934 = ORIENTED_EDGE ( 'NONE', *, *, #235, .F. ) ;
#10935 = ORIENTED_EDGE ( 'NONE', *, *, #6698, .F. ) ;
#10936 = CARTESIAN_POINT ( 'NONE',  ( 20.72575232321667116, 179.9202923768740732, -123.3302915314655479 ) ) ;
#10937 = EDGE_CURVE ( 'NONE', #2214, #1813, #196, .T. ) ;
#10938 = CARTESIAN_POINT ( 'NONE',  ( -19.87412339327474342, 180.5265370758251606, -122.4403904965001288 ) ) ;
#10939 = LINE ( 'NONE', #2526, #1461 ) ;
#10940 = CARTESIAN_POINT ( 'NONE',  ( -372.4159675733355357, 102.0139246166868077, -124.6604683294675766 ) ) ;
#10941 = CIRCLE ( 'NONE', #5613, 7.500000000000020428 ) ;
#10942 = CIRCLE ( 'NONE', #4239, 7.500000000000012434 ) ;
#10943 = CARTESIAN_POINT ( 'NONE',  ( -30.00000000000000000, -492.9999999999998863, -30.00000000000000000 ) ) ;
#10944 = AXIS2_PLACEMENT_3D ( 'NONE', #11827, #8972, #10771 ) ;
#10945 = DIRECTION ( 'NONE',  ( -0.000000000000000000, -1.000000000000000000, -1.757987137413040192E-14 ) ) ;
#10946 = DIRECTION ( 'NONE',  ( 0.000000000000000000, 1.000000000000000000, 0.000000000000000000 ) ) ;
#10947 = CARTESIAN_POINT ( 'NONE',  ( 0.000000000000000000, 24.00000000000001776, -124.6807709998038405 ) ) ;
#10948 = CARTESIAN_POINT ( 'NONE',  ( -157.5000000000000000, 24.00000000000001421, -126.4213562373084301 ) ) ;
#10949 = ORIENTED_EDGE ( 'NONE', *, *, #10921, .F. ) ;
#10950 = CARTESIAN_POINT ( 'NONE',  ( -1020.755281158171670, 68.40999151392655619, -149.7857175106638010 ) ) ;
#10951 = ORIENTED_EDGE ( 'NONE', *, *, #468, .T. ) ;
#10952 = CIRCLE ( 'NONE', #8593, 7.500000000000007994 ) ;
#10953 = AXIS2_PLACEMENT_3D ( 'NONE', #1568, #2375, #3732 ) ;
#10954 = CARTESIAN_POINT ( 'NONE',  ( -21.06231667407016772, 180.1636738665369251, -126.4297697749043010 ) ) ;
#10955 = DIRECTION ( 'NONE',  ( 0.000000000000000000, 0.000000000000000000, -1.000000000000000000 ) ) ;
#10956 = ORIENTED_EDGE ( 'NONE', *, *, #12209, .T. ) ;
#10957 = CARTESIAN_POINT ( 'NONE',  ( -372.6561862956065738, 62.83025961264725368, -118.7578631316695237 ) ) ;
#10958 = DIRECTION ( 'NONE',  ( -1.186840563529527301E-16, 1.000000000000000000, -0.000000000000000000 ) ) ;
#10959 = ORIENTED_EDGE ( 'NONE', *, *, #7525, .F. ) ;
#10960 = AXIS2_PLACEMENT_3D ( 'NONE', #8989, #4306, #8077 ) ;
#10961 = EDGE_LOOP ( 'NONE', ( #4174, #3454, #9284, #11979 ) ) ;
#10962 = CARTESIAN_POINT ( 'NONE',  ( -1014.132585063772808, 52.13780504951625261, -126.6442663926290777 ) ) ;
#10963 = LINE ( 'NONE', #3233, #4445 ) ;
#10964 = DIRECTION ( 'NONE',  ( -1.000000000000000000, -0.000000000000000000, -0.000000000000000000 ) ) ;
#10965 = DIRECTION ( 'NONE',  ( -0.000000000000000000, 1.000000000000000000, 7.930164461608263644E-17 ) ) ;
#10966 = CARTESIAN_POINT ( 'NONE',  ( -853.4539021257702416, 72.48584973915980356, -94.48732055948642028 ) ) ;
#10967 = DIRECTION ( 'NONE',  ( -1.000000000000000000, 0.000000000000000000, 0.000000000000000000 ) ) ;
#10968 = CARTESIAN_POINT ( 'NONE',  ( 8.937118865183852088E-16, 196.0000000000000000, -124.6807709998038405 ) ) ;
#10969 = ORIENTED_EDGE ( 'NONE', *, *, #2857, .F. ) ;
#10970 = CARTESIAN_POINT ( 'NONE',  ( -277.5000000000000000, 139.9999999999999716, -126.4213562373076059 ) ) ;
#10971 = EDGE_CURVE ( 'NONE', #6153, #6627, #10159, .T. ) ;
#10972 = DIRECTION ( 'NONE',  ( -1.186840563529527301E-16, 1.000000000000000000, -0.000000000000000000 ) ) ;
#10973 = ORIENTED_EDGE ( 'NONE', *, *, #3438, .F. ) ;
#10974 = DIRECTION ( 'NONE',  ( -0.000000000000000000, 1.000000000000000000, -0.000000000000000000 ) ) ;
#10976 = EDGE_CURVE ( 'NONE', #10559, #1936, #9956, .T. ) ;
#10975 = CARTESIAN_POINT ( 'NONE',  ( -955.9230626098324137, 78.80814421416175719, -95.06748246948052383 ) ) ;
#10977 = CARTESIAN_POINT ( 'NONE',  ( 120.8820948793965186, 12.00000000000000000, -179.1989091883332890 ) ) ;
#10978 = FACE_OUTER_BOUND ( 'NONE', #6487, .T. ) ;
#10979 = CARTESIAN_POINT ( 'NONE',  ( -20.77482174596494247, 180.9926187296578348, -123.5402880645763730 ) ) ;
#10980 = CIRCLE ( 'NONE', #3675, 7.500000000000007105 ) ;
#10981 = FACE_OUTER_BOUND ( 'NONE', #6412, .T. ) ;
#10982 = EDGE_CURVE ( 'NONE', #9219, #11532, #2995, .T. ) ;
#10983 = DIRECTION ( 'NONE',  ( 0.000000000000000000, 0.000000000000000000, 1.000000000000000000 ) ) ;
#10984 = CARTESIAN_POINT ( 'NONE',  ( -154.5043356068770493, 0.000000000000000000, -102.0666613060160302 ) ) ;
#10985 = FACE_BOUND ( 'NONE', #11034, .T. ) ;
#10986 = FACE_OUTER_BOUND ( 'NONE', #7722, .T. ) ;
#10987 = ORIENTED_EDGE ( 'NONE', *, *, #1799, .T. ) ;
#10988 = DIRECTION ( 'NONE',  ( -1.000000000000000000, -0.000000000000000000, -0.000000000000000000 ) ) ;
#10989 = CARTESIAN_POINT ( 'NONE',  ( -951.4444194419894529, 124.5703232071642503, -118.7903414690678829 ) ) ;
#10990 = DIRECTION ( 'NONE',  ( 0.000000000000000000, 1.000000000000000000, 0.000000000000000000 ) ) ;
#10991 = DIRECTION ( 'NONE',  ( -0.000000000000000000, 1.000000000000000000, 7.930164461608263644E-17 ) ) ;
#10992 = CARTESIAN_POINT ( 'NONE',  ( -7.499999999999998224, 24.00000000000001421, -126.4213562373094959 ) ) ;
#10993 = EDGE_CURVE ( 'NONE', #931, #10118, #6796, .T. ) ;
#10994 = CARTESIAN_POINT ( 'NONE',  ( 19.98378750576280538, 182.6226996931179087, -125.4995243108248388 ) ) ;
#10995 = EDGE_LOOP ( 'NONE', ( #5963, #5257 ) ) ;
#10996 = VECTOR ( 'NONE', #9466, 1000.000000000000000 ) ;
#10997 = ORIENTED_EDGE ( 'NONE', *, *, #5603, .T. ) ;
#10998 = CARTESIAN_POINT ( 'NONE',  ( -19.94337906914356395, 178.3983333771979858, -123.1706592317244144 ) ) ;
#10999 = CARTESIAN_POINT ( 'NONE',  ( -379.1619848709566440, 61.99999999999992184, -124.6807709998039542 ) ) ;
#11000 = CARTESIAN_POINT ( 'NONE',  ( -824.4897464405680694, 73.71539350114069578, -142.8842219741777342 ) ) ;
#11001 = CARTESIAN_POINT ( 'NONE',  ( 1.387778780781445676E-14, 0.000000000000000000, 126.4213562373094959 ) ) ;
#11002 = LINE ( 'NONE', #4456, #10932 ) ;
#11003 = CARTESIAN_POINT ( 'NONE',  ( -277.5000000000000000, 12.00000000000001066, -126.4213562373076059 ) ) ;
#11004 = EDGE_LOOP ( 'NONE', ( #6886, #1271, #4903, #10813 ) ) ;
#11005 = CARTESIAN_POINT ( 'NONE',  ( 0.000000000000000000, 0.000000000000000000, 0.000000000000000000 ) ) ;
#11006 = VECTOR ( 'NONE', #1941, 999.9999999999998863 ) ;
#11007 = EDGE_LOOP ( 'NONE', ( #12107, #11637, #8394, #2187 ) ) ;
#11008 = LINE ( 'NONE', #2838, #8447 ) ;
#11009 = CARTESIAN_POINT ( 'NONE',  ( -1032.391769651406321, 55.42093464310143247, -146.0307792196449839 ) ) ;
#11010 = ADVANCED_FACE ( 'NONE', ( #9428 ), #17, .F. ) ;
#11011 = CARTESIAN_POINT ( 'NONE',  ( 19.83177985141341892, 179.9887880572465519, -127.2693050255385714 ) ) ;
#11012 = VERTEX_POINT ( 'NONE', #1207 ) ;
#11013 = VECTOR ( 'NONE', #2642, 1000.000000000000000 ) ;
#11014 = LINE ( 'NONE', #5378, #4228 ) ;
#11015 = ORIENTED_EDGE ( 'NONE', *, *, #10779, .F. ) ;
#11016 = CARTESIAN_POINT ( 'NONE',  ( -369.8688452567520812, 55.69319535620513051, -124.6859973355406197 ) ) ;
#11017 = CARTESIAN_POINT ( 'NONE',  ( -6.360897667028196044E-14, -6.000000000000000000, -141.4213562373094817 ) ) ;
#11018 = EDGE_LOOP ( 'NONE', ( #3477, #8618, #7253, #8693 ) ) ;
#11019 = CIRCLE ( 'NONE', #5884, 7.500000000000020428 ) ;
#11020 = VERTEX_POINT ( 'NONE', #1949 ) ;
#11021 = CARTESIAN_POINT ( 'NONE',  ( -817.1493800258450619, 27.50875274330017461, -126.6442663926291630 ) ) ;
#11022 = AXIS2_PLACEMENT_3D ( 'NONE', #10807, #1358, #11681 ) ;
#11023 = FACE_OUTER_BOUND ( 'NONE', #7332, .T. ) ;
#11024 = CYLINDRICAL_SURFACE ( 'NONE', #8186, 5.999999999999999112 ) ;
#11025 = EDGE_CURVE ( 'NONE', #6366, #9074, #7394, .T. ) ;
#11026 = DIRECTION ( 'NONE',  ( 0.000000000000000000, 1.000000000000000000, 0.000000000000000000 ) ) ;
#11027 = AXIS2_PLACEMENT_3D ( 'NONE', #405, #8830, #10802 ) ;
#11028 = CARTESIAN_POINT ( 'NONE',  ( -1037.899050076301137, 86.18944477603540122, -95.06748246948046699 ) ) ;
#11029 = CARTESIAN_POINT ( 'NONE',  ( 126.4213562373094959, -6.000000000000000000, -6.938893903907228378E-15 ) ) ;
#11030 = CARTESIAN_POINT ( 'NONE',  ( 35.00000000000000000, 139.9999999999999716, -89.68077099980384048 ) ) ;
#11031 = ORIENTED_EDGE ( 'NONE', *, *, #1418, .T. ) ;
#11032 = CARTESIAN_POINT ( 'NONE',  ( -20.77322673479996951, 179.4133438526717441, -123.5311657466897373 ) ) ;
#11033 = DIRECTION ( 'NONE',  ( 0.000000000000000000, 0.000000000000000000, 1.000000000000000000 ) ) ;
#11034 = EDGE_LOOP ( 'NONE', ( #7008, #8218 ) ) ;
#11035 = CARTESIAN_POINT ( 'NONE',  ( -821.6111871957904214, 83.16774079293004718, -154.1944187633729939 ) ) ;
#11036 = CARTESIAN_POINT ( 'NONE',  ( -956.2104666674714508, 71.56905446038054208, -96.78565065507946485 ) ) ;
#11037 = DIRECTION ( 'NONE',  ( 0.000000000000000000, 0.000000000000000000, 1.000000000000000000 ) ) ;
#11038 = AXIS2_PLACEMENT_3D ( 'NONE', #1122, #4873, #8659 ) ;
#11039 = FACE_BOUND ( 'NONE', #8890, .T. ) ;
#11040 = CIRCLE ( 'NONE', #6114, 7.500000000000007105 ) ;
#11041 = FACE_OUTER_BOUND ( 'NONE', #11209, .T. ) ;
#11042 = EDGE_CURVE ( 'NONE', #6737, #368, #81, .T. ) ;
#11043 = CARTESIAN_POINT ( 'NONE',  ( -828.1717276517521213, 76.17609097696448828, -105.5454165443656507 ) ) ;
#11044 = CARTESIAN_POINT ( 'NONE',  ( -19.95913600371365959, 180.2478989036688972, -123.1890436974040313 ) ) ;
#11045 = CARTESIAN_POINT ( 'NONE',  ( -828.3261744505556408, 76.46613818254095918, -143.9024326026597294 ) ) ;
#11046 = ADVANCED_FACE ( 'NONE', ( #1161 ), #3994, .T. ) ;
#11047 = ORIENTED_EDGE ( 'NONE', *, *, #7129, .F. ) ;
#11048 = FACE_OUTER_BOUND ( 'NONE', #344, .T. ) ;
#11049 = CARTESIAN_POINT ( 'NONE',  ( -819.1467617552298179, 76.91148745156876032, -154.6757676722768906 ) ) ;
#11050 = ORIENTED_EDGE ( 'NONE', *, *, #4512, .T. ) ;
#11051 = DIRECTION ( 'NONE',  ( -0.3117078928809425831, -5.319854888938806247E-14, 0.9501779778103273122 ) ) ;
#11052 = CARTESIAN_POINT ( 'NONE',  ( -1024.691966601154036, 118.8493250655916142, -122.7172756069790580 ) ) ;
#11053 = CARTESIAN_POINT ( 'NONE',  ( -210.0000000000000000, 24.00000000000000711, -126.4213562373080180 ) ) ;
#11054 = DIRECTION ( 'NONE',  ( -0.000000000000000000, 1.000000000000000000, 0.000000000000000000 ) ) ;
#11055 = CARTESIAN_POINT ( 'NONE',  ( 0.000000000000000000, -494.9999999999998863, -118.9213562373094817 ) ) ;
#11056 = CARTESIAN_POINT ( 'NONE',  ( 20.96297238888044845, 181.6803933783718890, -124.5802004042857334 ) ) ;
#11057 = ORIENTED_EDGE ( 'NONE', *, *, #959, .T. ) ;
#11058 = EDGE_LOOP ( 'NONE', ( #5351, #3954, #3525, #7545 ) ) ;
#11059 = CARTESIAN_POINT ( 'NONE',  ( -1013.875822516560447, 120.2710389253235519, -124.6807709998039257 ) ) ;
#11060 = EDGE_CURVE ( 'NONE', #8373, #569, #6013, .T. ) ;
#11061 = FACE_OUTER_BOUND ( 'NONE', #3756, .T. ) ;
#11062 = CARTESIAN_POINT ( 'NONE',  ( -127.4999999999999716, 12.00000000000001421, -126.4213562373086575 ) ) ;
#11063 = CARTESIAN_POINT ( 'NONE',  ( -821.6815100408632588, 89.78153722040215712, -152.5758913445288840 ) ) ;
#11064 = CARTESIAN_POINT ( 'NONE',  ( -369.9371856203899824, 108.1376465818777177, -127.6226701653134796 ) ) ;
#11065 = EDGE_CURVE ( 'NONE', #966, #3468, #6207, .T. ) ;
#11066 = DIRECTION ( 'NONE',  ( 0.000000000000000000, 0.000000000000000000, 1.000000000000000000 ) ) ;
#11067 = DIRECTION ( 'NONE',  ( 0.000000000000000000, 1.000000000000000000, 0.000000000000000000 ) ) ;
#11068 = DIRECTION ( 'NONE',  ( 0.000000000000000000, 0.5000000000000018874, 0.8660254037844374864 ) ) ;
#11069 = ORIENTED_EDGE ( 'NONE', *, *, #1131, .F. ) ;
#11070 = PLANE ( 'NONE',  #5101 ) ;
#11071 = CARTESIAN_POINT ( 'NONE',  ( 1.387778780781445676E-14, -6.000000000000000000, 133.9213562373095101 ) ) ;
#11072 = EDGE_LOOP ( 'NONE', ( #10951, #1579 ) ) ;
#11073 = CARTESIAN_POINT ( 'NONE',  ( -89.99999999999998579, 24.00000000000001421, -126.4213562373088564 ) ) ;
#11074 = CARTESIAN_POINT ( 'NONE',  ( -1062.096538105497302, 73.81465972843197676, -154.2940595301284930 ) ) ;
#11075 = VERTEX_POINT ( 'NONE', #3119 ) ;
#11076 = ORIENTED_EDGE ( 'NONE', *, *, #11060, .F. ) ;
#11077 = FACE_OUTER_BOUND ( 'NONE', #698, .T. ) ;
#11078 = DIRECTION ( 'NONE',  ( -1.000000000000000000, 0.000000000000000000, -0.000000000000000000 ) ) ;
#11079 = ADVANCED_FACE ( 'NONE', ( #7762 ), #94, .F. ) ;
#11080 = ORIENTED_EDGE ( 'NONE', *, *, #3520, .T. ) ;
#11081 = EDGE_CURVE ( 'NONE', #11517, #8131, #10662, .T. ) ;
#11082 = CARTESIAN_POINT ( 'NONE',  ( -379.5247776001849616, 62.60840276516706382, -129.5872912034053286 ) ) ;
#11083 = CARTESIAN_POINT ( 'NONE',  ( -154.5043356068770493, 12.00000000000000000, -109.5666613060160586 ) ) ;
#11084 = VERTEX_POINT ( 'NONE', #3064 ) ;
#11085 = CYLINDRICAL_SURFACE ( 'NONE', #503, 7.499999999999992895 ) ;
#11086 = ORIENTED_EDGE ( 'NONE', *, *, #8213, .F. ) ;
#11087 = CARTESIAN_POINT ( 'NONE',  ( 6.257111856936825515E-13, -6.000000000000004441, -73.92135623730949590 ) ) ;
#11088 = CIRCLE ( 'NONE', #2016, 8.500000000000035527 ) ;
#11089 = DIRECTION ( 'NONE',  ( 0.000000000000000000, 1.000000000000000000, 0.000000000000000000 ) ) ;
#11090 = CARTESIAN_POINT ( 'NONE',  ( 19.98182870893229079, 179.3422780683628162, -125.8969293818015984 ) ) ;
#11091 = CARTESIAN_POINT ( 'NONE',  ( -927.2951026182247460, 99.13268410970638911, -95.06748246948001224 ) ) ;
#11092 = CARTESIAN_POINT ( 'NONE',  ( -126.4213562373094959, 0.000000000000000000, 2.255140518769849223E-14 ) ) ;
#11093 = DIRECTION ( 'NONE',  ( 0.000000000000000000, 1.788286221017408824E-14, -1.000000000000000000 ) ) ;
#11094 = CARTESIAN_POINT ( 'NONE',  ( -795.0000000000038654, 109.8950841424301359, -136.2353035311980136 ) ) ;
#11095 = CARTESIAN_POINT ( 'NONE',  ( -823.1761409384637318, 83.64233031452228317, -144.6133277457492170 ) ) ;
#11096 = CIRCLE ( 'NONE', #3789, 7.500000000000007105 ) ;
#11097 = ORIENTED_EDGE ( 'NONE', *, *, #6319, .T. ) ;
#11098 = CARTESIAN_POINT ( 'NONE',  ( -828.8285638327206470, 78.67432280806529832, -144.4023295390027215 ) ) ;
#11099 =( NAMED_UNIT ( * ) SI_UNIT ( $, .STERADIAN. ) SOLID_ANGLE_UNIT ( ) );
#11100 = EDGE_LOOP ( 'NONE', ( #435, #5638 ) ) ;
#11101 = CARTESIAN_POINT ( 'NONE',  ( -1056.743458481016432, 64.45745743522633120, -96.78565065507969223 ) ) ;
#11102 = CARTESIAN_POINT ( 'NONE',  ( 9.184850993605161750E-16, 0.000000000000000000, -133.9213562373095101 ) ) ;
#11103 = DIRECTION ( 'NONE',  ( 1.000000000000000000, -1.262554838833776231E-16, 0.000000000000000000 ) ) ;
#11104 = DIRECTION ( 'NONE',  ( 0.000000000000000000, 1.000000000000000000, 0.000000000000000000 ) ) ;
#11105 = CARTESIAN_POINT ( 'NONE',  ( 21.06333566525091072, 179.8959387247087705, -126.3976994828154545 ) ) ;
#11106 = CARTESIAN_POINT ( 'NONE',  ( 1.479627290717497352E-14, -58.00000000000000711, 118.9213562373094817 ) ) ;
#11107 = CIRCLE ( 'NONE', #2222, 7.500000000000020428 ) ;
#11108 = CARTESIAN_POINT ( 'NONE',  ( -826.0807747705194970, 74.19805998537496805, -106.2647609865421430 ) ) ;
#11109 = CARTESIAN_POINT ( 'NONE',  ( -19.99085265605563677, 178.9337235835365050, -123.8700625655956173 ) ) ;
#11110 = DIRECTION ( 'NONE',  ( -8.163404592832031500E-17, 1.000000000000000000, -0.000000000000000000 ) ) ;
#11111 = EDGE_LOOP ( 'NONE', ( #4898, #8676, #4111, #4617 ) ) ;
#11112 = ORIENTED_EDGE ( 'NONE', *, *, #2079, .F. ) ;
#11113 = CARTESIAN_POINT ( 'NONE',  ( -371.0428122657798440, 58.79643506041531964, -138.7203693468078427 ) ) ;
#11114 = CONTEXT_DEPENDENT_SHAPE_REPRESENTATION ( #10082, #8432 ) ;
#11115 = CARTESIAN_POINT ( 'NONE',  ( -904.1167769183923610, 122.8348148996190758, -136.2353035311977862 ) ) ;
#11116 = ORIENTED_EDGE ( 'NONE', *, *, #6619, .F. ) ;
#11117 = CARTESIAN_POINT ( 'NONE',  ( -926.5289067496665893, 125.3297071905304421, -118.7903414690680535 ) ) ;
#11118 = ADVANCED_FACE ( 'NONE', ( #10541 ), #6833, .F. ) ;
#11119 = CARTESIAN_POINT ( 'NONE',  ( 7.750278301654327006E-16, 197.0000000000000000, -124.6807709998038405 ) ) ;
#11120 = LINE ( 'NONE', #477, #3719 ) ;
#11121 = CARTESIAN_POINT ( 'NONE',  ( -372.9440792399824431, 65.15140800462232562, -101.6629770149452128 ) ) ;
#11122 = CARTESIAN_POINT ( 'NONE',  ( 19.98950317961507750, 182.6598950331495814, -125.3472100544021686 ) ) ;
#11123 = VECTOR ( 'NONE', #3618, 1000.000000000000000 ) ;
#11124 = VERTEX_POINT ( 'NONE', #8753 ) ;
#11125 = DIRECTION ( 'NONE',  ( 2.040851148208007875E-17, -1.000000000000000000, -0.000000000000000000 ) ) ;
#11126 = DIRECTION ( 'NONE',  ( -0.000000000000000000, -1.000000000000000000, -0.000000000000000000 ) ) ;
#11127 = CARTESIAN_POINT ( 'NONE',  ( -1014.911393615049064, 99.73439156315002663, -152.5758913445290261 ) ) ;
#11128 = CARTESIAN_POINT ( 'NONE',  ( -369.8859280133687548, 108.2643723699462726, -124.6535011946241127 ) ) ;
#11129 = DIRECTION ( 'NONE',  ( 1.000000000000000000, -1.026341648675396322E-47, 2.081668171172161734E-17 ) ) ;
#11130 = DIRECTION ( 'NONE',  ( 0.000000000000000000, 0.000000000000000000, 1.000000000000000000 ) ) ;
#11131 = CARTESIAN_POINT ( 'NONE',  ( -974.7984820115178763, 96.63273410478066694, -152.5758913445288272 ) ) ;
#11132 = DIRECTION ( 'NONE',  ( 0.000000000000000000, 0.000000000000000000, 1.000000000000000000 ) ) ;
#11133 = VERTEX_POINT ( 'NONE', #5032 ) ;
#11134 = DIRECTION ( 'NONE',  ( -1.000000000000000000, 0.000000000000000000, 0.000000000000000000 ) ) ;
#11135 = AXIS2_PLACEMENT_3D ( 'NONE', #8391, #4788, #5454 ) ;
#11136 = ADVANCED_FACE ( 'NONE', ( #8810 ), #2142, .F. ) ;
#11137 = ORIENTED_EDGE ( 'NONE', *, *, #9762, .T. ) ;
#11138 = CARTESIAN_POINT ( 'NONE',  ( -1065.000000000007958, 70.44548139156172795, -152.5758913445293388 ) ) ;
#11139 = ADVANCED_FACE ( 'NONE', ( #9677 ), #8572, .F. ) ;
#11140 = VERTEX_POINT ( 'NONE', #6711 ) ;
#11141 = ORIENTED_EDGE ( 'NONE', *, *, #3584, .T. ) ;
#11142 = CARTESIAN_POINT ( 'NONE',  ( 20.89973826391392464, 178.8616761932901795, -124.1694459372093178 ) ) ;
#11143 = AXIS2_PLACEMENT_3D ( 'NONE', #3267, #5304, #8161 ) ;
#11144 = EDGE_CURVE ( 'NONE', #7589, #6019, #4801, .T. ) ;
#11145 = VECTOR ( 'NONE', #781, 1000.000000000000000 ) ;
#11146 = CARTESIAN_POINT ( 'NONE',  ( -19.83893667468079869, 179.6461197167075170, -127.2139938056598965 ) ) ;
#11147 = AXIS2_PLACEMENT_3D ( 'NONE', #8698, #11599, #9555 ) ;
#11148 = ORIENTED_EDGE ( 'NONE', *, *, #3586, .F. ) ;
#11149 = DIRECTION ( 'NONE',  ( 0.000000000000000000, 1.000000000000000000, 0.000000000000000000 ) ) ;
#11150 = CARTESIAN_POINT ( 'NONE',  ( -373.4729226597870024, 66.15791503844970123, -136.9867814967885238 ) ) ;
#11151 = DIRECTION ( 'NONE',  ( -0.000000000000000000, -1.000000000000000000, 0.000000000000000000 ) ) ;
#11152 = VECTOR ( 'NONE', #6792, 1000.000000000000000 ) ;
#11153 = CYLINDRICAL_SURFACE ( 'NONE', #4444, 7.500000000000007105 ) ;
#11154 = EDGE_CURVE ( 'NONE', #8531, #11075, #4045, .T. ) ;
#11155 = DIRECTION ( 'NONE',  ( 0.000000000000000000, 0.000000000000000000, 1.000000000000000000 ) ) ;
#11156 = CARTESIAN_POINT ( 'NONE',  ( 19.89196810756490663, 178.6505532842396633, -126.7594064012678388 ) ) ;
#11157 = CARTESIAN_POINT ( 'NONE',  ( 1.249585401188644101E-12, 152.0000000000000000, 1.078643762690525199 ) ) ;
#11158 = CARTESIAN_POINT ( 'NONE',  ( -1047.626240907246483, 63.12837257276869707, -96.78565065507969223 ) ) ;
#11159 = DIRECTION ( 'NONE',  ( 0.000000000000000000, 0.000000000000000000, -1.000000000000000000 ) ) ;
#11160 = CARTESIAN_POINT ( 'NONE',  ( -379.1619848709566440, 61.99999999999992184, -124.6807709998039542 ) ) ;
#11161 = EDGE_CURVE ( 'NONE', #2093, #6037, #11659, .T. ) ;
#11162 = AXIS2_PLACEMENT_3D ( 'NONE', #4253, #12152, #7439 ) ;
#11163 = VECTOR ( 'NONE', #9754, 1000.000000000000000 ) ;
#11164 = ORIENTED_EDGE ( 'NONE', *, *, #10550, .F. ) ;
#11165 = FACE_BOUND ( 'NONE', #4240, .T. ) ;
#11166 = CARTESIAN_POINT ( 'NONE',  ( 214.0000708641547931, -3.383602624851756594E-13, 23.10407613178321640 ) ) ;
#11167 = CARTESIAN_POINT ( 'NONE',  ( -370.2377583643716434, 107.3781601596609221, -116.9922470894815945 ) ) ;
#11168 = ORIENTED_EDGE ( 'NONE', *, *, #10605, .T. ) ;
#11169 = CARTESIAN_POINT ( 'NONE',  ( 7.750278301654327006E-16, 197.0000000000000000, -124.6807709998038405 ) ) ;
#11170 = CARTESIAN_POINT ( 'NONE',  ( -853.7969483066802923, 45.36294356226295577, -99.57582448894520155 ) ) ;
#11171 = DIRECTION ( 'NONE',  ( 1.000000000000000000, 0.000000000000000000, 0.000000000000000000 ) ) ;
#11172 = DIRECTION ( 'NONE',  ( -1.000000000000000000, -1.186840563529527301E-16, 0.000000000000000000 ) ) ;
#11173 = CARTESIAN_POINT ( 'NONE',  ( 21.06244748020267465, 180.0923556010718869, -126.4260852699257356 ) ) ;
#11174 = ADVANCED_FACE ( 'NONE', ( #149 ), #3177, .F. ) ;
#11175 = CARTESIAN_POINT ( 'NONE',  ( -29.99999999999998934, 24.00000000000001421, -126.4213562373092685 ) ) ;
#11176 = VECTOR ( 'NONE', #11344, 999.9999999999998863 ) ;
#11177 = CARTESIAN_POINT ( 'NONE',  ( -828.8285638327206470, 78.67432280806529832, -104.9592124606049879 ) ) ;
#11178 = CARTESIAN_POINT ( 'NONE',  ( -20.73637609554099726, 179.7535993509491163, -123.3744064433501677 ) ) ;
#11179 = CARTESIAN_POINT ( 'NONE',  ( -828.8285638327209881, 78.51036871773257531, -144.3746817048997855 ) ) ;
#11180 = ORIENTED_EDGE ( 'NONE', *, *, #3885, .T. ) ;
#11181 = EDGE_LOOP ( 'NONE', ( #10637, #2715, #7409, #6464 ) ) ;
#11182 = CARTESIAN_POINT ( 'NONE',  ( -370.2814337190545189, 56.73344489815470126, -132.8949611453235491 ) ) ;
#11183 = CARTESIAN_POINT ( 'NONE',  ( -371.4445559945335162, 104.0267551742128660, -108.3548430067642698 ) ) ;
#11184 = DIRECTION ( 'NONE',  ( -0.000000000000000000, -1.000000000000000000, -0.000000000000000000 ) ) ;
#11185 = AXIS2_PLACEMENT_3D ( 'NONE', #6430, #5306, #10200 ) ;
#11186 = ORIENTED_EDGE ( 'NONE', *, *, #1007, .T. ) ;
#11187 = CARTESIAN_POINT ( 'NONE',  ( -904.1167769183953169, 122.8348148996191611, -113.1262384684093263 ) ) ;
#11188 = CIRCLE ( 'NONE', #1317, 7.500000000000007105 ) ;
#11189 = CARTESIAN_POINT ( 'NONE',  ( 141.4213562373095101, -494.9999999999998863, -1.508194112741312283E-14 ) ) ;
#11190 = DIRECTION ( 'NONE',  ( -0.000000000000000000, 1.000000000000000000, 7.930164461608263644E-17 ) ) ;
#11191 = CARTESIAN_POINT ( 'NONE',  ( 19.99966070409250207, 182.7093770945723463, -124.8756968753967271 ) ) ;
#11192 = ORIENTED_EDGE ( 'NONE', *, *, #10025, .F. ) ;
#11193 = AXIS2_PLACEMENT_3D ( 'NONE', #1896, #3799, #11596 ) ;
#11194 = ORIENTED_EDGE ( 'NONE', *, *, #1984, .F. ) ;
#11195 = VECTOR ( 'NONE', #8914, 1000.000000000000000 ) ;
#11196 = APPLICATION_CONTEXT ( 'automotive_design' ) ;
#11197 = CARTESIAN_POINT ( 'NONE',  ( -29.95840947131392795, 180.2041921146317236, -138.2654117679345802 ) ) ;
#11198 = CARTESIAN_POINT ( 'NONE',  ( 6.899999999999999467, 0.000000000000000000, 0.000000000000000000 ) ) ;
#11199 = CARTESIAN_POINT ( 'NONE',  ( -994.1998135634695473, 88.30642396300672203, -154.2940595301282656 ) ) ;
#11200 = CARTESIAN_POINT ( 'NONE',  ( -370.2978394803209881, 107.2231406293463749, -116.3573562623202235 ) ) ;
#11201 = DIRECTION ( 'NONE',  ( -1.000000000000000000, -8.163404592832031500E-17, 0.000000000000000000 ) ) ;
#11202 = DIRECTION ( 'NONE',  ( -1.000000000000000000, 0.000000000000000000, 0.000000000000000000 ) ) ;
#11203 = VERTEX_POINT ( 'NONE', #3870 ) ;
#11204 = DIRECTION ( 'NONE',  ( -0.000000000000000000, -1.000000000000000000, -0.000000000000000000 ) ) ;
#11205 = CARTESIAN_POINT ( 'NONE',  ( -382.9619892260665210, 93.96448540389030768, -140.7106330510814303 ) ) ;
#11206 = VERTEX_POINT ( 'NONE', #7703 ) ;
#11207 = CARTESIAN_POINT ( 'NONE',  ( -1038.028607166442953, 78.75533988487831039, -154.8742214401230797 ) ) ;
#11208 = CIRCLE ( 'NONE', #11788, 7.500000000000007105 ) ;
#11209 = EDGE_LOOP ( 'NONE', ( #5148, #5917, #5749, #10973 ) ) ;
#11210 = EDGE_LOOP ( 'NONE', ( #4845, #1992, #2945, #3182 ) ) ;
#11211 = EDGE_CURVE ( 'NONE', #11690, #8735, #2266, .T. ) ;
#11212 = CARTESIAN_POINT ( 'NONE',  ( -19.96713961980339391, 182.4999670356679076, -125.8362662571105517 ) ) ;
#11213 = CARTESIAN_POINT ( 'NONE',  ( -828.1717276517556456, 76.17609097696481513, -105.5454165443659491 ) ) ;
#11214 = AXIS2_PLACEMENT_3D ( 'NONE', #9700, #7975, #8939 ) ;
#11215 = ADVANCED_FACE ( 'NONE', ( #2259 ), #2020, .T. ) ;
#11216 = ORIENTED_EDGE ( 'NONE', *, *, #4745, .T. ) ;
#11217 = AXIS2_PLACEMENT_3D ( 'NONE', #2494, #7327, #11159 ) ;
#11218 = CARTESIAN_POINT ( 'NONE',  ( -379.4788071961805827, 62.53013482031470716, -129.2670437572034245 ) ) ;
#11219 = CYLINDRICAL_SURFACE ( 'NONE', #10319, 7.500000000000013323 ) ;
#11220 = CARTESIAN_POINT ( 'NONE',  ( 4.808665244885994618E-14, -494.9999999999998863, 141.4213562373094817 ) ) ;
#11221 = VERTEX_POINT ( 'NONE', #6267 ) ;
#11222 = DIRECTION ( 'NONE',  ( 0.000000000000000000, 1.000000000000000000, -0.000000000000000000 ) ) ;
#11223 = MECHANICAL_DESIGN_GEOMETRIC_PRESENTATION_REPRESENTATION (  '', ( #751 ), #5877 ) ;
#11224 = CARTESIAN_POINT ( 'NONE',  ( 6.247927005943220505E-13, 152.0000000000000000, -66.42135623730948168 ) ) ;
#11225 = FACE_OUTER_BOUND ( 'NONE', #9818, .T. ) ;
#11226 = CARTESIAN_POINT ( 'NONE',  ( -1021.293373424897709, 59.24127555818995461, -107.9061927053327281 ) ) ;
#11227 = LINE ( 'NONE', #3407, #8248 ) ;
#11228 = DIRECTION ( 'NONE',  ( 0.000000000000000000, 0.000000000000000000, 1.000000000000000000 ) ) ;
#11229 = CARTESIAN_POINT ( 'NONE',  ( -379.4314023685043935, 101.5510643398535393, -129.0327286575446806 ) ) ;
#11230 = AXIS2_PLACEMENT_3D ( 'NONE', #2331, #4877, #5165 ) ;
#11231 = VERTEX_POINT ( 'NONE', #8979 ) ;
#11232 =( GEOMETRIC_REPRESENTATION_CONTEXT ( 3 ) GLOBAL_UNCERTAINTY_ASSIGNED_CONTEXT ( ( #6955 ) ) GLOBAL_UNIT_ASSIGNED_CONTEXT ( ( #1676, #10078, #10140 ) ) REPRESENTATION_CONTEXT ( 'NONE', 'WORKASPACE' ) );
#11233 = EDGE_CURVE ( 'NONE', #8803, #6402, #9168, .T. ) ;
#11234 = DIRECTION ( 'NONE',  ( 0.9994711065474020106, -9.540873247276913062E-16, -0.03251933543158296025 ) ) ;
#11235 = FILL_AREA_STYLE ('',( #7450 ) ) ;
#11236 = EDGE_LOOP ( 'NONE', ( #241, #8646, #7137, #6381 ) ) ;
#11237 = CARTESIAN_POINT ( 'NONE',  ( -141.4213562373095101, -6.000000000000000000, 3.644282033693712520E-14 ) ) ;
#11238 = CARTESIAN_POINT ( 'NONE',  ( -1057.036663358159558, 58.23757105449750071, -99.57582448894497418 ) ) ;
#11239 = CARTESIAN_POINT ( 'NONE',  ( -1065.000000000006366, 82.00000000000036948, -124.6807709998044231 ) ) ;
#11240 = CARTESIAN_POINT ( 'NONE',  ( -112.4999999999999716, 12.00000000000001421, -126.4213562373086575 ) ) ;
#11241 = PLANE ( 'NONE',  #1034 ) ;
#11242 = AXIS2_PLACEMENT_3D ( 'NONE', #9000, #5984, #8883 ) ;
#11243 = AXIS2_PLACEMENT_3D ( 'NONE', #5135, #3387, #8049 ) ;
#11244 = CARTESIAN_POINT ( 'NONE',  ( 1.874378101782966050E-12, -6.000000000000006217, 61.07864376269051121 ) ) ;
#11245 = CARTESIAN_POINT ( 'NONE',  ( -20.74457341359024198, 179.6607161185452810, -123.4086842481865602 ) ) ;
#11246 = DIRECTION ( 'NONE',  ( -1.000000000000000000, 0.000000000000000000, 0.000000000000000000 ) ) ;
#11247 = ORIENTED_EDGE ( 'NONE', *, *, #10064, .T. ) ;
#11248 = FACE_OUTER_BOUND ( 'NONE', #5494, .T. ) ;
#11249 = EDGE_CURVE ( 'NONE', #2061, #11517, #7790, .T. ) ;
#11250 = MECHANICAL_DESIGN_GEOMETRIC_PRESENTATION_REPRESENTATION (  '', ( #5300 ), #982 ) ;
#11251 = ORIENTED_EDGE ( 'NONE', *, *, #6820, .T. ) ;
#11252 = CARTESIAN_POINT ( 'NONE',  ( -1037.550865396562358, 105.7975851359348241, -103.3307627799636350 ) ) ;
#11253 = CYLINDRICAL_SURFACE ( 'NONE', #6485, 7.500000000000007105 ) ;
#11254 = CARTESIAN_POINT ( 'NONE',  ( 19.98725602524029554, 182.5262326453932076, -123.9529870253308133 ) ) ;
#11255 = ORIENTED_EDGE ( 'NONE', *, *, #4496, .T. ) ;
#11256 = AXIS2_PLACEMENT_3D ( 'NONE', #6838, #9440, #977 ) ;
#11257 = EDGE_LOOP ( 'NONE', ( #5272, #6100 ) ) ;
#11258 = CARTESIAN_POINT ( 'NONE',  ( -29.99999999999998579, 12.00000000000001776, -126.4213562373092685 ) ) ;
#11259 = DIRECTION ( 'NONE',  ( 0.7071067811865473507, 0.000000000000000000, -0.7071067811865477948 ) ) ;
#11260 = LINE ( 'NONE', #12057, #6196 ) ;
#11261 = CARTESIAN_POINT ( 'NONE',  ( -1037.899050076299318, 86.18944477603574228, -154.2940595301282656 ) ) ;
#11262 = VERTEX_POINT ( 'NONE', #3470 ) ;
#11263 = DIRECTION ( 'NONE',  ( -0.000000000000000000, -0.000000000000000000, -1.000000000000000000 ) ) ;
#11264 = CARTESIAN_POINT ( 'NONE',  ( -373.4495655788976478, 96.65560026510921432, -149.5745928868048793 ) ) ;
#11265 = ORIENTED_EDGE ( 'NONE', *, *, #7971, .F. ) ;
#11266 = CARTESIAN_POINT ( 'NONE',  ( -927.4753839990684128, 92.66010094724849466, -154.8742214401223691 ) ) ;
#11267 = CARTESIAN_POINT ( 'NONE',  ( 19.90078111156755014, 181.8690955493196384, -126.6770338381014938 ) ) ;
#11268 = VERTEX_POINT ( 'NONE', #9912 ) ;
#11269 = VERTEX_POINT ( 'NONE', #439 ) ;
#11270 = CARTESIAN_POINT ( 'NONE',  ( 4.285787411236815022E-15, 24.00000000000001776, -126.4213562373094959 ) ) ;
#11271 = CARTESIAN_POINT ( 'NONE',  ( -1032.503061859593117, 50.81309391744441228, -141.4553492942758908 ) ) ;
#11272 = CARTESIAN_POINT ( 'NONE',  ( -372.7454185398722757, 64.37420824858371304, -146.9174072618011451 ) ) ;
#11273 = CYLINDRICAL_SURFACE ( 'NONE', #1435, 7.500000000000007105 ) ;
#11274 = CARTESIAN_POINT ( 'NONE',  ( -373.0607415668539488, 65.63369181740749525, -101.2204817476631149 ) ) ;
#11275 = DIRECTION ( 'NONE',  ( 0.000000000000000000, 0.000000000000000000, 1.000000000000000000 ) ) ;
#11276 = ORIENTED_EDGE ( 'NONE', *, *, #6542, .F. ) ;
#11277 = EDGE_CURVE ( 'NONE', #11012, #9215, #7130, .T. ) ;
#11278 = DIRECTION ( 'NONE',  ( 0.000000000000000000, 0.000000000000000000, -1.000000000000000000 ) ) ;
#11279 = CARTESIAN_POINT ( 'NONE',  ( 45.53315400109643463, 12.00000000000000000, -237.8419396193597208 ) ) ;
#11280 = CARTESIAN_POINT ( 'NONE',  ( -1027.375436305349467, 71.63039521860197567, -96.78565065507956433 ) ) ;
#11281 = CARTESIAN_POINT ( 'NONE',  ( -819.8468830326183934, 81.71630402067619059, -104.6809196082603961 ) ) ;
#11282 = CARTESIAN_POINT ( 'NONE',  ( -1062.996098538724254, 47.98024286075312261, -130.5712005305402101 ) ) ;
#11283 = VERTEX_POINT ( 'NONE', #1441 ) ;
#11284 = CARTESIAN_POINT ( 'NONE',  ( -828.1678681009874481, 81.16376924194455000, -144.6638077543058785 ) ) ;
#11285 = CARTESIAN_POINT ( 'NONE',  ( 178.4695970358725674, 1.116338468047439712E-13, -54.32942441097565478 ) ) ;
#11286 = EDGE_LOOP ( 'NONE', ( #7330, #2781, #11408, #3631 ) ) ;
#11287 = CIRCLE ( 'NONE', #27, 1.499999999999999112 ) ;
#11288 = CARTESIAN_POINT ( 'NONE',  ( -1025.595947590972401, 58.17469240935120922, -107.9061927053327707 ) ) ;
#11289 = DIRECTION ( 'NONE',  ( -1.000000000000000000, -0.000000000000000000, -6.195440985631455317E-17 ) ) ;
#11290 = EDGE_CURVE ( 'NONE', #11808, #5900, #278, .T. ) ;
#11291 = CARTESIAN_POINT ( 'NONE',  ( -19.03136272649511085, 180.2041921146316668, -134.6807709998038547 ) ) ;
#11292 = CARTESIAN_POINT ( 'NONE',  ( -20.71964524312745937, 180.2041921146310415, -123.3053720114591272 ) ) ;
#11293 = AXIS2_PLACEMENT_3D ( 'NONE', #2426, #10964, #11953 ) ;
#11294 = EDGE_LOOP ( 'NONE', ( #3702, #1807, #748, #4393 ) ) ;
#11295 = CARTESIAN_POINT ( 'NONE',  ( 126.4213562373094959, -494.9999999999998863, -6.938893903907228378E-15 ) ) ;
#11296 = CARTESIAN_POINT ( 'NONE',  ( -373.4631759638398307, 96.59209656397271715, -99.73825686774256383 ) ) ;
#11297 = ORIENTED_EDGE ( 'NONE', *, *, #9288, .T. ) ;
#11298 = CARTESIAN_POINT ( 'NONE',  ( -1065.000000000008868, 103.3499740386314016, -103.3307627799635924 ) ) ;
#11299 = DIRECTION ( 'NONE',  ( 0.000000000000000000, 1.689469820081754479E-14, -1.000000000000000000 ) ) ;
#11300 = CARTESIAN_POINT ( 'NONE',  ( -823.8285638327238303, 78.67432280806536937, -89.68077099980398259 ) ) ;
#11301 = AXIS2_PLACEMENT_3D ( 'NONE', #8319, #6511, #4473 ) ;
#11302 = EDGE_CURVE ( 'NONE', #1954, #10270, #2260, .T. ) ;
#11303 = ADVANCED_FACE ( 'NONE', ( #10895 ), #11024, .T. ) ;
#11304 = CARTESIAN_POINT ( 'NONE',  ( -1054.380968608932108, 114.0683136310379524, -122.7172756069792570 ) ) ;
#11305 = VERTEX_POINT ( 'NONE', #11889 ) ;
#11306 = CARTESIAN_POINT ( 'NONE',  ( -926.5138833012647410, 125.7648744980332225, -124.6807709998040394 ) ) ;
#11307 = CARTESIAN_POINT ( 'NONE',  ( 154.5043356068769071, 12.00000000000000000, -102.0666613060171386 ) ) ;
#11308 = LINE ( 'NONE', #678, #3426 ) ;
#11309 = CARTESIAN_POINT ( 'NONE',  ( -1019.017691546887363, 99.44610047464912839, -152.5758913445291967 ) ) ;
#11310 = TOROIDAL_SURFACE ( 'NONE', #5978, 8.500000000000003553, 1.000000000000000000 ) ;
#11311 = EDGE_CURVE ( 'NONE', #8172, #206, #1284, .T. ) ;
#11312 = EDGE_CURVE ( 'NONE', #7974, #2536, #6998, .T. ) ;
#11313 = CARTESIAN_POINT ( 'NONE',  ( -27.99999999999999645, -492.9999999999998863, 27.99999999999999645 ) ) ;
#11314 = ORIENTED_EDGE ( 'NONE', *, *, #789, .F. ) ;
#11315 = CARTESIAN_POINT ( 'NONE',  ( -374.3697334861134323, 92.69272124223820697, -141.6596876525885307 ) ) ;
#11316 = ORIENTED_EDGE ( 'NONE', *, *, #9688, .F. ) ;
#11317 = CARTESIAN_POINT ( 'NONE',  ( -853.6888141844391384, 53.84495383942815039, -152.5758913445293103 ) ) ;
#11318 = AXIS2_PLACEMENT_3D ( 'NONE', #5482, #10184, #8282 ) ;
#11319 = DIRECTION ( 'NONE',  ( 1.000000000000000000, 0.000000000000000000, 0.000000000000000000 ) ) ;
#11320 = ORIENTED_EDGE ( 'NONE', *, *, #11065, .F. ) ;
#11321 = ADVANCED_FACE ( 'NONE', ( #7194 ), #7201, .T. ) ;
#11322 = EDGE_LOOP ( 'NONE', ( #7321, #2560, #3073, #7062 ) ) ;
#11323 = DIRECTION ( 'NONE',  ( -0.000000000000000000, -1.000000000000000000, -0.000000000000000000 ) ) ;
#11324 = CARTESIAN_POINT ( 'NONE',  ( -828.3259789886610633, 76.46577308275233520, -105.4592182070451543 ) ) ;
#11325 = CARTESIAN_POINT ( 'NONE',  ( -818.8285638327206470, 78.67432280806529832, -144.4023295390026931 ) ) ;
#11326 = CARTESIAN_POINT ( 'NONE',  ( -1048.206790403134164, 45.99070412075050740, -141.4553492942756918 ) ) ;
#11327 = VECTOR ( 'NONE', #11367, 1000.000000000000000 ) ;
#11328 = ORIENTED_EDGE ( 'NONE', *, *, #9932, .T. ) ;
#11329 = CARTESIAN_POINT ( 'NONE',  ( -374.9564170155092597, 84.61582091868922362, -154.5477554669674305 ) ) ;
#11330 = CYLINDRICAL_SURFACE ( 'NONE', #4398, 1.500000000000000444 ) ;
#11331 = DIRECTION ( 'NONE',  ( 0.000000000000000000, 1.000000000000000000, 0.000000000000000000 ) ) ;
#11332 = CIRCLE ( 'NONE', #461, 7.500000000000007105 ) ;
#11333 = CIRCLE ( 'NONE', #4823, 7.500000000000007105 ) ;
#11334 = FACE_OUTER_BOUND ( 'NONE', #9664, .T. ) ;
#11335 = CARTESIAN_POINT ( 'NONE',  ( -1047.844889418690855, 56.55730854968127375, -99.57582448894520155 ) ) ;
#11336 = CARTESIAN_POINT ( 'NONE',  ( -824.1545993022754146, 83.67440335600112178, -104.7509849144500578 ) ) ;
#11337 = CARTESIAN_POINT ( 'NONE',  ( -1025.943122242211757, 53.12767954719351593, -130.5712005305404375 ) ) ;
#11338 = LINE ( 'NONE', #7754, #7951 ) ;
#11339 = EDGE_LOOP ( 'NONE', ( #6515, #7530, #10873, #1248 ) ) ;
#11340 = CARTESIAN_POINT ( 'NONE',  ( -827.6030183929041186, 81.96987526947627600, -144.6820941065182069 ) ) ;
#11341 = AXIS2_PLACEMENT_3D ( 'NONE', #648, #10104, #1637 ) ;
#11342 = PRODUCT_CONTEXT ( 'NONE', #6132, 'mechanical' ) ;
#11343 = AXIS2_PLACEMENT_3D ( 'NONE', #10408, #5711, #8560 ) ;
#11344 = DIRECTION ( 'NONE',  ( 0.7071067811865473507, 0.000000000000000000, -0.7071067811865477948 ) ) ;
#11345 = CARTESIAN_POINT ( 'NONE',  ( 126.4213562373094959, -492.9999999999998863, -6.938893903907228378E-15 ) ) ;
#11346 = VERTEX_POINT ( 'NONE', #6208 ) ;
#11347 = CARTESIAN_POINT ( 'NONE',  ( -853.8938961404153360, 37.86297855175766358, -103.3307627799636776 ) ) ;
#11348 = DIRECTION ( 'NONE',  ( 1.000000000000000000, 2.040851148208007875E-17, 0.000000000000000000 ) ) ;
#11349 = CARTESIAN_POINT ( 'NONE',  ( 0.5612050131712165157, 4.355613924429928119, -9.000000000000001776 ) ) ;
#11350 = CARTESIAN_POINT ( 'NONE',  ( 19.98008256664037674, 179.4972950632025857, -125.9865773177933477 ) ) ;
#11351 = PRODUCT_DEFINITION_CONTEXT ( 'detailed design', #11822, 'design' ) ;
#11352 = CIRCLE ( 'NONE', #8407, 35.00000000000000000 ) ;
#11353 = DIRECTION ( 'NONE',  ( 0.000000000000000000, -1.000000000000000000, -7.930164461608263644E-17 ) ) ;
#11354 = CARTESIAN_POINT ( 'NONE',  ( -19.99764744648923909, 178.7270483677477841, -125.0101186568579266 ) ) ;
#11355 = DIRECTION ( 'NONE',  ( -8.163404592832030268E-17, 1.000000000000000000, -0.000000000000000000 ) ) ;
#11356 = EDGE_CURVE ( 'NONE', #10880, #3561, #508, .T. ) ;
#11357 = ORIENTED_EDGE ( 'NONE', *, *, #10927, .F. ) ;
#11358 = CARTESIAN_POINT ( 'NONE',  ( -374.5812891589289961, 89.65635038802255963, -95.98092888736175610 ) ) ;
#11359 = EDGE_CURVE ( 'NONE', #3156, #7498, #10963, .T. ) ;
#11360 = ORIENTED_EDGE ( 'NONE', *, *, #11364, .T. ) ;
#11361 = CARTESIAN_POINT ( 'NONE',  ( -1014.382386707157252, 110.5980896718282196, -103.3307627799636350 ) ) ;
#11362 = DIRECTION ( 'NONE',  ( -0.000000000000000000, -1.000000000000000000, -1.757987137413040192E-14 ) ) ;
#11363 = CARTESIAN_POINT ( 'NONE',  ( -363.0000000000000568, 81.99999999999995737, -89.68077099980384048 ) ) ;
#11364 = EDGE_CURVE ( 'NONE', #11808, #6290, #7067, .T. ) ;
#11365 = CARTESIAN_POINT ( 'NONE',  ( -1065.000000000007731, 112.0000000000007105, -122.7172756069790438 ) ) ;
#11366 = ORIENTED_EDGE ( 'NONE', *, *, #6220, .F. ) ;
#11367 = DIRECTION ( 'NONE',  ( -1.000000000000000000, -0.000000000000000000, -0.000000000000000000 ) ) ;
#11368 = AXIS2_PLACEMENT_3D ( 'NONE', #4586, #5243, #615 ) ;
#11369 = CARTESIAN_POINT ( 'NONE',  ( -828.8285638327206470, 78.67432280806529832, -264.6807709998040536 ) ) ;
#11370 = FACE_BOUND ( 'NONE', #10088, .T. ) ;
#11371 = CARTESIAN_POINT ( 'NONE',  ( -903.6727718957008619, 110.0506089609179838, -149.7857175106632326 ) ) ;
#11372 = LINE ( 'NONE', #1921, #1463 ) ;
#11373 = CYLINDRICAL_SURFACE ( 'NONE', #2089, 45.00000000000000711 ) ;
#11374 = ORIENTED_EDGE ( 'NONE', *, *, #11, .T. ) ;
#11375 = EDGE_CURVE ( 'NONE', #8373, #1329, #3854, .T. ) ;
#11376 = CARTESIAN_POINT ( 'NONE',  ( -374.2771194692035692, 92.15366326334435598, -152.4146676682642010 ) ) ;
#11377 = PRODUCT_DEFINITION_SHAPE ( 'NONE', 'NONE',  #7149 ) ;
#11378 = CARTESIAN_POINT ( 'NONE',  ( -19.97506881502268428, 181.0839254472395510, -123.4722291287969114 ) ) ;
#11379 = FACE_BOUND ( 'NONE', #5263, .T. ) ;
#11380 = ORIENTED_EDGE ( 'NONE', *, *, #7228, .T. ) ;
#11381 = AXIS2_PLACEMENT_3D ( 'NONE', #5018, #4161, #7876 ) ;
#11382 = VERTEX_POINT ( 'NONE', #577 ) ;
#11383 = CARTESIAN_POINT ( 'NONE',  ( 19.90629981715767016, 178.9629118261667600, -122.7457835946827913 ) ) ;
#11384 = CARTESIAN_POINT ( 'NONE',  ( -21.06303090563296365, 181.4372473149129803, -125.7691643379808255 ) ) ;
#11385 = CARTESIAN_POINT ( 'NONE',  ( -383.1580143002730665, 93.38886992431909562, -141.1315691075368193 ) ) ;
#11386 = DIRECTION ( 'NONE',  ( 0.000000000000000000, 0.000000000000000000, 1.000000000000000000 ) ) ;
#11387 = CARTESIAN_POINT ( 'NONE',  ( -996.5513353153702383, 56.29506814688406990, -149.7857175106634600 ) ) ;
#11388 = VERTEX_POINT ( 'NONE', #5330 ) ;
#11389 = CARTESIAN_POINT ( 'NONE',  ( -384.9501908748870278, 83.99300641423289449, -144.5920939778981733 ) ) ;
#11390 = CARTESIAN_POINT ( 'NONE',  ( -305.0000000000000568, 24.00000000000000711, -89.68077099980384048 ) ) ;
#11391 = CARTESIAN_POINT ( 'NONE',  ( -374.7441414241753819, 75.96258608733518258, -95.46849099916960313 ) ) ;
#11392 = VECTOR ( 'NONE', #10239, 1000.000000000000000 ) ;
#11394 = EDGE_CURVE ( 'NONE', #1000, #3418, #12151, .T. ) ;
#11393 = LINE ( 'NONE', #2931, #147 ) ;
#11395 = CARTESIAN_POINT ( 'NONE',  ( -997.7839878466141954, 40.27522178589210711, -136.2353035311988378 ) ) ;
#11396 = ORIENTED_EDGE ( 'NONE', *, *, #8809, .T. ) ;
#11397 = CARTESIAN_POINT ( 'NONE',  ( -29.99999999999998579, -9.213203435596451385, -126.4213562373092685 ) ) ;
#11398 = VECTOR ( 'NONE', #4237, 1000.000000000000000 ) ;
#11399 = CARTESIAN_POINT ( 'NONE',  ( -1021.046747802643722, 63.38047825189596551, -103.3307627799639761 ) ) ;
#11400 = CARTESIAN_POINT ( 'NONE',  ( -818.8285638327243987, 79.00074005404812283, -104.9041682110414371 ) ) ;
#11401 = CARTESIAN_POINT ( 'NONE',  ( 7.500000000000000000, 5.196152422706624030, -9.000000000000000000 ) ) ;
#11402 = ORIENTED_EDGE ( 'NONE', *, *, #6446, .F. ) ;
#11403 = CARTESIAN_POINT ( 'NONE',  ( -381.8446789258243825, 67.15007266234491112, -111.2347306979282848 ) ) ;
#11404 = DIRECTION ( 'NONE',  ( -0.000000000000000000, 1.000000000000000000, 7.930164461608263644E-17 ) ) ;
#11405 = ORIENTED_EDGE ( 'NONE', *, *, #10485, .T. ) ;
#11406 = APPLICATION_PROTOCOL_DEFINITION ( 'draft international standard', 'automotive_design', 1998, #7158 ) ;
#11407 = SURFACE_STYLE_FILL_AREA ( #11235 ) ;
#11408 = ORIENTED_EDGE ( 'NONE', *, *, #2215, .F. ) ;
#11409 = CARTESIAN_POINT ( 'NONE',  ( -1038.401083800584274, 57.54275223462379074, -99.57582448894500260 ) ) ;
#11410 = CARTESIAN_POINT ( 'NONE',  ( -823.8285638327242850, 78.67432280806536937, -90.68077099980378364 ) ) ;
#11411 = B_SPLINE_CURVE_WITH_KNOTS ( 'NONE', 3,
 ( #7510, #11400, #10347, #2937, #6701, #11463, #8688, #11281, #6583, #1891, #16, #5653, #1149, #6823, #195, #2132, #10474, #8507, #138, #11336, #12213, #9606, #9427, #3980, #8455, #3921, #3793, #2009, #9543, #7749, #963, #5890, #7690, #2994, #7567, #2877, #6755, #4791 ),
 .UNSPECIFIED., .F., .F.,
 ( 4, 2, 2, 2, 2, 2, 2, 2, 2, 2, 2, 2, 2, 2, 2, 2, 2, 2, 4 ),
 ( 0.000000000000000000, 0.0009791294386042174221, 0.001958258877208434844, 0.002937388315812651616, 0.003916517754416869689, 0.004895647193021087328, 0.005874776631625303232, 0.006364341350927419858, 0.006853906070229536483, 0.007833035508834094995, 0.008812164947438654375, 0.009791294386043212020, 0.01077042382464777140, 0.01174955326325232731, 0.01272868270185688495, 0.01370781214046144433, 0.01468694157906600198, 0.01517650629836831376, 0.01566607101767062554 ),
 .UNSPECIFIED. ) ;
#11412 = DIRECTION ( 'NONE',  ( 0.000000000000000000, 1.000000000000000000, 0.000000000000000000 ) ) ;
#11413 = CARTESIAN_POINT ( 'NONE',  ( -1014.170783943992433, 114.7803637426472534, -107.9061927053325292 ) ) ;
#11414 = PLANE ( 'NONE',  #7899 ) ;
#11415 = CARTESIAN_POINT ( 'NONE',  ( 0.000000000000000000, 0.000000000000000000, 0.000000000000000000 ) ) ;
#11416 = AXIS2_PLACEMENT_3D ( 'NONE', #5419, #4447, #1536 ) ;
#11417 = ORIENTED_EDGE ( 'NONE', *, *, #10666, .T. ) ;
#11418 = CARTESIAN_POINT ( 'NONE',  ( -126.4213562373094959, 0.000000000000000000, 7.500000000000035527 ) ) ;
#11419 = CARTESIAN_POINT ( 'NONE',  ( -382.7045174276864259, 94.69426221061047499, -109.2122950466990829 ) ) ;
#11420 = VERTEX_POINT ( 'NONE', #5150 ) ;
#11421 = CARTESIAN_POINT ( 'NONE',  ( -853.0139081111171890, 107.1087209265617020, -103.3307627799635355 ) ) ;
#11422 = AXIS2_PLACEMENT_3D ( 'NONE', #2947, #1837, #9438 ) ;
#11423 = DIRECTION ( 'NONE',  ( -1.000000000000000000, 0.000000000000000000, -6.195440985631454085E-17 ) ) ;
#11424 = CARTESIAN_POINT ( 'NONE',  ( -180.0000000000000000, -9.213203435596478030, -126.4213562373082453 ) ) ;
#11425 = AXIS2_PLACEMENT_3D ( 'NONE', #10947, #9774, #8961 ) ;
#11426 = ADVANCED_FACE ( 'NONE', ( #10838 ), #10039, .F. ) ;
#11427 = CARTESIAN_POINT ( 'NONE',  ( -1024.691966601152672, 118.8493250655916142, -124.6807709998039400 ) ) ;
#11428 = ORIENTED_EDGE ( 'NONE', *, *, #9645, .F. ) ;
#11429 = DIRECTION ( 'NONE',  ( 0.000000000000000000, 0.000000000000000000, 1.000000000000000000 ) ) ;
#11430 = CYLINDRICAL_SURFACE ( 'NONE', #8720, 7.500000000000007105 ) ;
#11431 = CARTESIAN_POINT ( 'NONE',  ( -87.04832655144203102, 12.00000000000000000, -217.9289243767376831 ) ) ;
#11432 = CARTESIAN_POINT ( 'NONE',  ( -954.5323978148076094, 113.6695689568733911, -146.0307792196442165 ) ) ;
#11433 = LINE ( 'NONE', #2967, #11930 ) ;
#11434 = CARTESIAN_POINT ( 'NONE',  ( 6.247927005943220505E-13, -6.000000000000006217, -58.92135623730948879 ) ) ;
#11435 = EDGE_LOOP ( 'NONE', ( #1436, #951 ) ) ;
#11436 = CARTESIAN_POINT ( 'NONE',  ( 1.562900236585165577E-12, -6.000000000000004441, 16.07864376269049700 ) ) ;
#11437 = CARTESIAN_POINT ( 'NONE',  ( -379.7887390581964837, 100.9343252097582422, -131.1221473163307678 ) ) ;
#11438 = CARTESIAN_POINT ( 'NONE',  ( -954.5323978148076094, 113.6695689568733911, -146.0307792196442165 ) ) ;
#11439 = AXIS2_PLACEMENT_3D ( 'NONE', #9517, #936, #4709 ) ;
#11440 = AXIS2_PLACEMENT_3D ( 'NONE', #7908, #8879, #6044 ) ;
#11441 = DIRECTION ( 'NONE',  ( -1.000000000000000000, -0.000000000000000000, -0.000000000000000000 ) ) ;
#11442 = EDGE_CURVE ( 'NONE', #1342, #7207, #7323, .T. ) ;
#11443 = ORIENTED_EDGE ( 'NONE', *, *, #11311, .T. ) ;
#11444 = VERTEX_POINT ( 'NONE', #4041 ) ;
#11445 = CARTESIAN_POINT ( 'NONE',  ( 19.98289417481194974, 179.1164216503652540, -123.6441077975231480 ) ) ;
#11446 = DIRECTION ( 'NONE',  ( -0.000000000000000000, 1.000000000000000000, 1.669238443041288415E-16 ) ) ;
#11447 = CARTESIAN_POINT ( 'NONE',  ( -19.99909886256255476, 181.7106308440128544, -124.9041157096212800 ) ) ;
#11448 = CARTESIAN_POINT ( 'NONE',  ( -305.0000000000000568, 12.00000000000001066, -89.68077099980384048 ) ) ;
#11449 = CARTESIAN_POINT ( 'NONE',  ( -1032.260242496265846, 61.00429285198246987, -149.7857175106635452 ) ) ;
#11450 = ADVANCED_FACE ( 'NONE', ( #5950 ), #5001, .F. ) ;
#11451 = CARTESIAN_POINT ( 'NONE',  ( -374.9532740794444408, 85.24015211620390176, -144.4367336822883203 ) ) ;
#11452 = DIRECTION ( 'NONE',  ( 0.000000000000000000, 0.000000000000000000, -1.000000000000000000 ) ) ;
#11453 = CARTESIAN_POINT ( 'NONE',  ( -372.4851915888308440, 63.39452537575517255, -103.4953678669831731 ) ) ;
#11454 = CARTESIAN_POINT ( 'NONE',  ( 35.00000000000000000, 12.00000000000001954, -124.6807709998040110 ) ) ;
#11455 = EDGE_LOOP ( 'NONE', ( #9269, #12161, #6441, #3879 ) ) ;
#11456 = CARTESIAN_POINT ( 'NONE',  ( -976.2351830774960035, 35.86345807843989775, -130.5712005305402101 ) ) ;
#11457 = ORIENTED_EDGE ( 'NONE', *, *, #903, .F. ) ;
#11458 = EDGE_CURVE ( 'NONE', #3561, #1856, #8595, .T. ) ;
#11459 = EDGE_CURVE ( 'NONE', #11527, #4090, #7800, .T. ) ;
#11460 = DIRECTION ( 'NONE',  ( -0.000000000000000000, 1.000000000000000000, 7.930164461608263644E-17 ) ) ;
#11461 = EDGE_CURVE ( 'NONE', #8369, #6191, #3422, .T. ) ;
#11462 = CARTESIAN_POINT ( 'NONE',  ( -1013.637332661006667, 62.09754518945625534, -103.3307627799637913 ) ) ;
#11463 = CARTESIAN_POINT ( 'NONE',  ( -819.3307005430699519, 80.88259174529733286, -104.7097040407758328 ) ) ;
#11464 = DIRECTION ( 'NONE',  ( 1.000000000000000000, 0.000000000000000000, 0.000000000000000000 ) ) ;
#11465 = ORIENTED_EDGE ( 'NONE', *, *, #6843, .T. ) ;
#11466 = CARTESIAN_POINT ( 'NONE',  ( -383.3096726399348881, 92.91657833282617673, -107.9127011693687592 ) ) ;
#11467 = ORIENTED_EDGE ( 'NONE', *, *, #1316, .F. ) ;
#11468 = CARTESIAN_POINT ( 'NONE',  ( 126.4213562373094959, -492.9999999999998863, 7.500000000000006217 ) ) ;
#11469 = ORIENTED_EDGE ( 'NONE', *, *, #1462, .F. ) ;
#11470 = EDGE_CURVE ( 'NONE', #7883, #5923, #8783, .T. ) ;
#11471 = CARTESIAN_POINT ( 'NONE',  ( 6.899999999999999467, 0.000000000000000000, 0.000000000000000000 ) ) ;
#11472 = SHAPE_DEFINITION_REPRESENTATION ( #11377, #4488 ) ;
#11473 = EDGE_LOOP ( 'NONE', ( #9738, #3562, #6130, #1283 ) ) ;
#11474 = CARTESIAN_POINT ( 'NONE',  ( -928.3598895237944362, 61.90886769853011629, -113.1262384684093831 ) ) ;
#11475 = CARTESIAN_POINT ( 'NONE',  ( -52.49999999999997868, -9.213203435596451385, -126.4213562373090696 ) ) ;
#11476 = DIRECTION ( 'NONE',  ( 1.000000000000000000, 0.000000000000000000, 0.000000000000000000 ) ) ;
#11477 = PRODUCT_DEFINITION_CONTEXT ( 'detailed design', #7158, 'design' ) ;
#11478 = ADVANCED_FACE ( 'NONE', ( #10005 ), #4578, .F. ) ;
#11479 = DIRECTION ( 'NONE',  ( -1.000000000000000000, 0.000000000000000000, 0.000000000000000000 ) ) ;
#11480 = VERTEX_POINT ( 'NONE', #541 ) ;
#11481 = PRODUCT_DEFINITION_SHAPE ( 'NONE', 'NONE',  #3143 ) ;
#11482 = DIRECTION ( 'NONE',  ( 2.081668171172161734E-17, 4.930380657631307143E-31, -1.000000000000000000 ) ) ;
#11483 = CARTESIAN_POINT ( 'NONE',  ( -374.9244159347675236, 86.03385731159455929, -105.0706672234830279 ) ) ;
#11484 = ORIENTED_EDGE ( 'NONE', *, *, #944, .F. ) ;
#11485 = CARTESIAN_POINT ( 'NONE',  ( -1065.000000000002956, 98.77454568802522772, -99.57582448894488891 ) ) ;
#11486 = FACE_OUTER_BOUND ( 'NONE', #7417, .T. ) ;
#11487 = CARTESIAN_POINT ( 'NONE',  ( -1045.967528061855091, 112.8272211019271225, -136.2353035311980705 ) ) ;
#11488 = AXIS2_PLACEMENT_3D ( 'NONE', #8632, #3932, #148 ) ;
#11489 = DIRECTION ( 'NONE',  ( 0.000000000000000000, -1.000000000000000000, -0.000000000000000000 ) ) ;
#11490 = ORIENTED_EDGE ( 'NONE', *, *, #6855, .F. ) ;
#11491 = LINE ( 'NONE', #6786, #4416 ) ;
#11492 = DIRECTION ( 'NONE',  ( -8.163404592832030268E-17, 1.000000000000000000, -0.000000000000000000 ) ) ;
#11493 = CARTESIAN_POINT ( 'NONE',  ( 9.371890508914830252E-13, 12.00000000000000000, -36.42135623730949590 ) ) ;
#11494 = CARTESIAN_POINT ( 'NONE',  ( -1022.396981161619806, 109.5926079579672603, -146.0307792196444154 ) ) ;
#11495 = DIRECTION ( 'NONE',  ( 0.000000000000000000, 0.000000000000000000, -1.000000000000000000 ) ) ;
#11496 = LINE ( 'NONE', #2380, #87 ) ;
#11497 = ORIENTED_EDGE ( 'NONE', *, *, #5846, .T. ) ;
#11498 = AXIS2_PLACEMENT_3D ( 'NONE', #10692, #9889, #1422 ) ;
#11499 = FACE_OUTER_BOUND ( 'NONE', #7366, .T. ) ;
#11500 = CARTESIAN_POINT ( 'NONE',  ( -1018.692594135740137, 105.1726068785159214, -149.7857175106633747 ) ) ;
#11501 = FACE_BOUND ( 'NONE', #11072, .T. ) ;
#11502 = ORIENTED_EDGE ( 'NONE', *, *, #10330, .F. ) ;
#11503 = DIRECTION ( 'NONE',  ( -1.000000000000000000, 0.000000000000000000, 0.000000000000000000 ) ) ;
#11504 = ORIENTED_EDGE ( 'NONE', *, *, #6937, .T. ) ;
#11505 = VECTOR ( 'NONE', #5262, 1000.000000000000000 ) ;
#11506 = DIRECTION ( 'NONE',  ( -3.061276722312011504E-17, 1.000000000000000000, 0.000000000000000000 ) ) ;
#11507 = CARTESIAN_POINT ( 'NONE',  ( 1.250503886288004501E-12, 0.000000000000000000, -13.92135623730950300 ) ) ;
#11508 = CARTESIAN_POINT ( 'NONE',  ( -1065.000000000007958, 70.44548139156172795, -152.5758913445293388 ) ) ;
#11509 = ORIENTED_EDGE ( 'NONE', *, *, #8944, .T. ) ;
#11510 = ADVANCED_FACE ( 'NONE', ( #606 ), #8351, .F. ) ;
#11511 = CARTESIAN_POINT ( 'NONE',  ( -384.9881694512860122, 81.02463022630767853, -144.6597318544169468 ) ) ;
#11512 = DIRECTION ( 'NONE',  ( 0.000000000000000000, 0.000000000000000000, -1.000000000000000000 ) ) ;
#11513 = CARTESIAN_POINT ( 'NONE',  ( -372.3192185535621661, 62.80464693345950877, -104.1946045324745143 ) ) ;
#11514 = EDGE_CURVE ( 'NONE', #7370, #10150, #9176, .T. ) ;
#11515 = CARTESIAN_POINT ( 'NONE',  ( 6.257111856936825515E-13, -6.000000000000004441, -73.92135623730949590 ) ) ;
#11516 = DIRECTION ( 'NONE',  ( 0.000000000000000000, -1.000000000000000000, -7.930164461608263644E-17 ) ) ;
#11517 = VERTEX_POINT ( 'NONE', #11055 ) ;
#11518 = CARTESIAN_POINT ( 'NONE',  ( -901.8967518049312275, 57.00804855647886171, -130.5712005305400965 ) ) ;
#11519 = VERTEX_POINT ( 'NONE', #7165 ) ;
#11520 = EDGE_CURVE ( 'NONE', #9670, #6223, #12047, .T. ) ;
#11521 = AXIS2_PLACEMENT_3D ( 'NONE', #6592, #11104, #6338 ) ;
#11522 = CARTESIAN_POINT ( 'NONE',  ( -956.9243412622536198, 54.10650223846825924, -107.9061927053324439 ) ) ;
#11523 = DIRECTION ( 'NONE',  ( 0.000000000000000000, -1.000000000000000000, -4.625929269271452387E-16 ) ) ;
#11524 = CARTESIAN_POINT ( 'NONE',  ( -1062.923339974281134, 49.86928741160674150, -136.2353035311989515 ) ) ;
#11525 = ORIENTED_EDGE ( 'NONE', *, *, #1545, .F. ) ;
#11526 = CARTESIAN_POINT ( 'NONE',  ( -380.8706770098667675, 65.08321416438575113, -113.9963688427722133 ) ) ;
#11527 = VERTEX_POINT ( 'NONE', #3626 ) ;
#11528 = FACE_OUTER_BOUND ( 'NONE', #2048, .T. ) ;
#11529 = EDGE_LOOP ( 'NONE', ( #7416, #4049, #8910, #6488 ) ) ;
#11530 = CARTESIAN_POINT ( 'NONE',  ( 1.562900236585165577E-12, 163.9999999999999716, 16.07864376269051121 ) ) ;
#11531 = SHAPE_DEFINITION_REPRESENTATION ( #1126, #12068 ) ;
#11532 = VERTEX_POINT ( 'NONE', #10992 ) ;
#11533 = CARTESIAN_POINT ( 'NONE',  ( -795.0000000000061391, 52.38665522077228331, -118.7903414690680250 ) ) ;
#11534 = VECTOR ( 'NONE', #7384, 1000.000000000000000 ) ;
#11535 = EDGE_CURVE ( 'NONE', #7471, #11763, #9768, .T. ) ;
#11536 = LINE ( 'NONE', #6832, #5096 ) ;
#11537 = VECTOR ( 'NONE', #6305, 1000.000000000000000 ) ;
#11538 = DIRECTION ( 'NONE',  ( 0.000000000000000000, 0.000000000000000000, 1.000000000000000000 ) ) ;
#11539 = FACE_OUTER_BOUND ( 'NONE', #3517, .T. ) ;
#11540 = PRODUCT_DEFINITION ( 'UNKNOWN', '', #10386, #10486 ) ;
#11541 = CARTESIAN_POINT ( 'NONE',  ( -954.3284336448667773, 118.5422944683823800, -107.9061927053323302 ) ) ;
#11542 = CARTESIAN_POINT ( 'NONE',  ( -305.0000000000000568, 81.99999999999995737, -159.6807709998038547 ) ) ;
#11543 = CARTESIAN_POINT ( 'NONE',  ( 151.3258811035896656, 12.00000000000000000, -56.13263083939798292 ) ) ;
#11544 = CIRCLE ( 'NONE', #2257, 11.50000000000001066 ) ;
#11545 = AXIS2_PLACEMENT_3D ( 'NONE', #1514, #5276, #9050 ) ;
#11546 = ORIENTED_EDGE ( 'NONE', *, *, #7658, .T. ) ;
#11547 = AXIS2_PLACEMENT_3D ( 'NONE', #4913, #3008, #2948 ) ;
#11548 = ORIENTED_EDGE ( 'NONE', *, *, #3959, .F. ) ;
#11549 = CARTESIAN_POINT ( 'NONE',  ( -1012.226803665789134, 93.06815595962675047, -95.06748246948018277 ) ) ;
#11550 = EDGE_CURVE ( 'NONE', #8380, #7767, #6652, .T. ) ;
#11551 = ORIENTED_EDGE ( 'NONE', *, *, #1229, .F. ) ;
#11552 = VECTOR ( 'NONE', #5895, 1000.000000000000000 ) ;
#11553 = CARTESIAN_POINT ( 'NONE',  ( 19.90865200055593220, 181.4799304009739558, -122.7714319726113104 ) ) ;
#11554 = AXIS2_PLACEMENT_3D ( 'NONE', #10690, #2226, #9942 ) ;
#11555 = DIRECTION ( 'NONE',  ( -0.000000000000000000, 1.000000000000000000, 7.930164461608263644E-17 ) ) ;
#11556 = ORIENTED_EDGE ( 'NONE', *, *, #9846, .T. ) ;
#11557 = CARTESIAN_POINT ( 'NONE',  ( -821.3208927675245832, 83.01261617297987527, -104.7055743826751524 ) ) ;
#11558 = CYLINDRICAL_SURFACE ( 'NONE', #5108, 7.500000000000007105 ) ;
#11559 = CARTESIAN_POINT ( 'NONE',  ( -823.1749794181308744, 110.1592441374104112, -141.4553492942763171 ) ) ;
#11560 = DIRECTION ( 'NONE',  ( -0.3117078928809153826, -1.979053562451413181E-14, -0.9501779778103363050 ) ) ;
#11561 = CARTESIAN_POINT ( 'NONE',  ( 126.4213562373094959, -494.9999999999998863, -6.938893903907228378E-15 ) ) ;
#11562 = CIRCLE ( 'NONE', #7616, 45.00000000000001421 ) ;
#11563 = CARTESIAN_POINT ( 'NONE',  ( 6.899999999999999467, 5.196152422706624918, 8.999999999999998224 ) ) ;
#11564 =( NAMED_UNIT ( * ) SI_UNIT ( $, .STERADIAN. ) SOLID_ANGLE_UNIT ( ) );
#11565 = EDGE_LOOP ( 'NONE', ( #1873, #4850 ) ) ;
#11566 = CARTESIAN_POINT ( 'NONE',  ( -1045.864486809339724, 115.5688325305733741, -124.6807709998043663 ) ) ;
#11567 = CARTESIAN_POINT ( 'NONE',  ( 6.276229776741093196E-15, 138.9999999999999716, -171.4213562373095101 ) ) ;
#11568 = DIRECTION ( 'NONE',  ( 0.000000000000000000, -0.000000000000000000, 1.000000000000000000 ) ) ;
#11569 = ORIENTED_EDGE ( 'NONE', *, *, #9408, .F. ) ;
#11570 = PLANE ( 'NONE',  #4298 ) ;
#11571 = EDGE_LOOP ( 'NONE', ( #380, #2522, #5137, #8018 ) ) ;
#11572 = CARTESIAN_POINT ( 'NONE',  ( -382.1799076831810567, 96.06408218159914725, -138.9468483416044080 ) ) ;
#11573 = CARTESIAN_POINT ( 'NONE',  ( -976.0610374937396045, 42.74778062430040393, -141.4553492942756634 ) ) ;
#11574 = CARTESIAN_POINT ( 'NONE',  ( -87.04832655144203102, 12.00000000000000000, -217.9289243767376831 ) ) ;
#11575 = DIRECTION ( 'NONE',  ( -1.000000000000000000, -0.000000000000000000, -0.000000000000000000 ) ) ;
#11576 = PLANE ( 'NONE',  #7562 ) ;
#11577 = SURFACE_STYLE_USAGE ( .BOTH. , #9718 ) ;
#11578 = PRODUCT_DEFINITION_FORMATION_WITH_SPECIFIED_SOURCE ( 'ANY', '', #12175, .NOT_KNOWN. ) ;
#11579 = CYLINDRICAL_SURFACE ( 'NONE', #11778, 35.00000000000000000 ) ;
#11580 = AXIS2_PLACEMENT_3D ( 'NONE', #12043, #4377, #1958 ) ;
#11581 = ORIENTED_EDGE ( 'NONE', *, *, #2840, .F. ) ;
#11582 = ADVANCED_FACE ( 'NONE', ( #10931 ), #2519, .T. ) ;
#11583 = PRODUCT_DEFINITION_SHAPE ( 'NONE', 'NONE',  #12246 ) ;
#11584 = VERTEX_POINT ( 'NONE', #2461 ) ;
#11585 = CARTESIAN_POINT ( 'NONE',  ( -828.8285638327245124, 78.67432280806571043, -264.6807709998050200 ) ) ;
#11586 = EDGE_CURVE ( 'NONE', #9164, #3075, #8097, .T. ) ;
#11587 = CARTESIAN_POINT ( 'NONE',  ( -1048.334963668458158, 42.40858384259915681, -113.1262384684096105 ) ) ;
#11588 = CARTESIAN_POINT ( 'NONE',  ( -19.83523559361558242, 180.6327028742894640, -127.2433017073463759 ) ) ;
#11589 = CARTESIAN_POINT ( 'NONE',  ( -957.1839320239870403, 48.17551948191491817, -130.5712005305400112 ) ) ;
#11590 = EDGE_LOOP ( 'NONE', ( #122, #11141 ) ) ;
#11591 = CIRCLE ( 'NONE', #11978, 5.000000000000115463 ) ;
#11592 = APPLICATION_CONTEXT ( 'automotive_design' ) ;
#11593 = CARTESIAN_POINT ( 'NONE',  ( -382.9953213592942802, 93.87473434840769926, -108.5770281898287237 ) ) ;
#11594 = CARTESIAN_POINT ( 'NONE',  ( 1.249585401188644101E-12, 164.0000000000000000, -6.421356237309481685 ) ) ;
#11595 = ORIENTED_EDGE ( 'NONE', *, *, #3136, .F. ) ;
#11596 = DIRECTION ( 'NONE',  ( 0.000000000000000000, -1.000000000000000000, 0.000000000000000000 ) ) ;
#11597 = ORIENTED_EDGE ( 'NONE', *, *, #782, .F. ) ;
#11598 = CARTESIAN_POINT ( 'NONE',  ( -998.0431609429222135, 37.14019503514177956, -122.7172756069792854 ) ) ;
#11599 = DIRECTION ( 'NONE',  ( -1.186840563529527301E-16, 1.000000000000000000, -0.000000000000000000 ) ) ;
#11600 = DIRECTION ( 'NONE',  ( -0.000000000000000000, 1.000000000000000000, 7.930164461608263644E-17 ) ) ;
#11601 = VECTOR ( 'NONE', #11892, 999.9999999999998863 ) ;
#11602 = EDGE_CURVE ( 'NONE', #11305, #7589, #906, .T. ) ;
#11603 = CARTESIAN_POINT ( 'NONE',  ( -1046.457602311629898, 98.67849639484570901, -99.57582448894517313 ) ) ;
#11604 = CARTESIAN_POINT ( 'NONE',  ( 0.000000000000000000, -6.000000000000000000, -118.9213562373094817 ) ) ;
#11605 = DIRECTION ( 'NONE',  ( -1.186840563529527301E-16, 1.000000000000000000, -0.000000000000000000 ) ) ;
#11606 = ADVANCED_FACE ( 'NONE', ( #6239 ), #8290, .F. ) ;
#11607 = ORIENTED_EDGE ( 'NONE', *, *, #3033, .T. ) ;
#11608 = CARTESIAN_POINT ( 'NONE',  ( 9.371890508914830252E-13, 12.00000000000000000, -28.92135623730948524 ) ) ;
#11609 = AXIS2_PLACEMENT_3D ( 'NONE', #7437, #2873, #7503 ) ;
#11610 = EDGE_CURVE ( 'NONE', #5923, #7883, #2082, .T. ) ;
#11611 = CARTESIAN_POINT ( 'NONE',  ( 144.0488662551573782, 12.00000000000000000, -146.9077238332702109 ) ) ;
#11612 = VERTEX_POINT ( 'NONE', #3386 ) ;
#11613 = CARTESIAN_POINT ( 'NONE',  ( -1055.469533842434430, 91.91071092603658599, -96.78565065507918064 ) ) ;
#11614 = EDGE_LOOP ( 'NONE', ( #5598, #85, #201, #810 ) ) ;
#11615 = CARTESIAN_POINT ( 'NONE',  ( -1037.392967692951970, 114.2240391150264998, -136.2353035311982126 ) ) ;
#11616 = DIRECTION ( 'NONE',  ( 1.000000000000000000, -1.262554838833776231E-16, 0.000000000000000000 ) ) ;
#11617 = LINE ( 'NONE', #2210, #4961 ) ;
#11618 = CARTESIAN_POINT ( 'NONE',  ( -926.5289067496665893, 125.3297071905304421, -118.7903414690680535 ) ) ;
#11619 = EDGE_LOOP ( 'NONE', ( #4945, #4066, #5547, #9675 ) ) ;
#11620 = EDGE_CURVE ( 'NONE', #3812, #4792, #2459, .T. ) ;
#11621 = CARTESIAN_POINT ( 'NONE',  ( -19.97946249231785032, 182.4386859306654856, -123.7598397378640556 ) ) ;
#11622 = ADVANCED_FACE ( 'NONE', ( #11869 ), #1802, .F. ) ;
#11623 = CARTESIAN_POINT ( 'NONE',  ( 7.653191805780027529E-16, 138.9999999999999716, -126.4213562373094959 ) ) ;
#11624 = DIRECTION ( 'NONE',  ( 0.000000000000000000, 0.000000000000000000, 1.000000000000000000 ) ) ;
#11625 = CARTESIAN_POINT ( 'NONE',  ( 20.84205126700888400, 179.0243517598608776, -123.8490133567502340 ) ) ;
#11626 = VECTOR ( 'NONE', #854, 1000.000000000000000 ) ;
#11627 = LINE ( 'NONE', #10681, #12160 ) ;
#11628 = ORIENTED_EDGE ( 'NONE', *, *, #4269, .T. ) ;
#11629 = CARTESIAN_POINT ( 'NONE',  ( -370.4401466759219375, 106.8513018378076964, -134.3428354745942102 ) ) ;
#11630 = CIRCLE ( 'NONE', #10038, 7.500000000000007105 ) ;
#11631 = FACE_OUTER_BOUND ( 'NONE', #10745, .T. ) ;
#11632 = CARTESIAN_POINT ( 'NONE',  ( -1011.211222789229396, 114.9684118750914621, -141.4553492942763455 ) ) ;
#11633 = CARTESIAN_POINT ( 'NONE',  ( 1.387778780781445676E-14, -58.00000000000000711, 126.4213562373094959 ) ) ;
#11634 = CARTESIAN_POINT ( 'NONE',  ( -112.4999999999999716, -9.213203435596451385, -126.4213562373086575 ) ) ;
#11635 = EDGE_LOOP ( 'NONE', ( #1204, #3229, #11255, #2305 ) ) ;
#11636 = CIRCLE ( 'NONE', #9258, 9.000000000000000000 ) ;
#11637 = ORIENTED_EDGE ( 'NONE', *, *, #5332, .T. ) ;
#11638 = CARTESIAN_POINT ( 'NONE',  ( -384.9187498600809931, 84.67419646485878104, -144.5370176048736539 ) ) ;
#11639 = CARTESIAN_POINT ( 'NONE',  ( -795.0000000000011369, 65.22545431197602284, -149.7857175106635452 ) ) ;
#11640 = CARTESIAN_POINT ( 'NONE',  ( -819.4840074578181657, 76.17856360854504771, -143.8168744253326565 ) ) ;
#11641 = CARTESIAN_POINT ( 'NONE',  ( -374.6737801889016168, 88.75927878213079225, -153.6720828349020849 ) ) ;
#11642 = DIRECTION ( 'NONE',  ( -1.000000000000000000, -0.000000000000000000, -0.000000000000000000 ) ) ;
#11643 = LINE ( 'NONE', #8793, #10811 ) ;
#11644 = CIRCLE ( 'NONE', #11440, 6.599999999999998757 ) ;
#11645 = ORIENTED_EDGE ( 'NONE', *, *, #6373, .T. ) ;
#11646 = EDGE_LOOP ( 'NONE', ( #6139, #1747, #3700, #358 ) ) ;
#11647 = CARTESIAN_POINT ( 'NONE',  ( -1025.806732200646138, 55.05754055295012961, -113.1262384684095537 ) ) ;
#11648 = FACE_OUTER_BOUND ( 'NONE', #6898, .T. ) ;
#11649 = ORIENTED_EDGE ( 'NONE', *, *, #7228, .F. ) ;
#11650 = CARTESIAN_POINT ( 'NONE',  ( -379.3727436124818269, 62.35000097320466494, -120.7242238939077339 ) ) ;
#11651 = DIRECTION ( 'NONE',  ( 1.186840563529527301E-16, -1.000000000000000000, 0.000000000000000000 ) ) ;
#11652 = ORIENTED_EDGE ( 'NONE', *, *, #11842, .F. ) ;
#11653 = CARTESIAN_POINT ( 'NONE',  ( -826.0420070959999066, 74.18794025998390396, -154.6674632209163178 ) ) ;
#11654 = EDGE_LOOP ( 'NONE', ( #3340, #8182 ) ) ;
#11655 = ADVANCED_FACE ( 'NONE', ( #11997 ), #7304, .F. ) ;
#11656 = VERTEX_POINT ( 'NONE', #4458 ) ;
#11657 = CARTESIAN_POINT ( 'NONE',  ( -1063.013736978594579, 47.55218547899811199, -126.6442663926291914 ) ) ;
#11658 = CARTESIAN_POINT ( 'NONE',  ( 126.4213562373094959, -494.9999999999998863, -6.938893903907228378E-15 ) ) ;
#11659 = LINE ( 'NONE', #8633, #5615 ) ;
#11660 = UNCERTAINTY_MEASURE_WITH_UNIT (LENGTH_MEASURE( 1.000000000000000082E-05 ), #752, 'distance_accuracy_value', 'NONE');
#11661 = DIRECTION ( 'NONE',  ( 0.000000000000000000, 0.000000000000000000, 1.000000000000000000 ) ) ;
#11662 = CARTESIAN_POINT ( 'NONE',  ( -822.2439855206088168, 97.57287547056382948, -99.57582448894494576 ) ) ;
#11663 = LINE ( 'NONE', #6957, #7649 ) ;
#11664 = CARTESIAN_POINT ( 'NONE',  ( 2.186774452080127126E-12, 152.0000000000000000, 83.57864376269051832 ) ) ;
#11665 = ORIENTED_EDGE ( 'NONE', *, *, #2317, .F. ) ;
#11666 = SHAPE_REPRESENTATION_RELATIONSHIP ( 'NONE' , 'NONE' ,  #2032, #8841 ) ;
#11667 = EDGE_CURVE ( 'NONE', #7054, #5440, #8968, .T. ) ;
#11668 = ORIENTED_EDGE ( 'NONE', *, *, #8586, .F. ) ;
#11669 = ADVANCED_FACE ( 'NONE', ( #8365 ), #5504, .F. ) ;
#11671 = EDGE_CURVE ( 'NONE', #6366, #3468, #9279, .T. ) ;
#11670 = CARTESIAN_POINT ( 'NONE',  ( -903.2629211055218548, 97.63080833215146015, -95.06748246947979908 ) ) ;
#11672 = VERTEX_POINT ( 'NONE', #4527 ) ;
#11673 = CARTESIAN_POINT ( 'NONE',  ( -1030.944970944897250, 117.4714819019839354, -130.5712005305406649 ) ) ;
#11674 = CARTESIAN_POINT ( 'NONE',  ( -795.0000000000035243, 112.0000000000008953, -126.6442663926293477 ) ) ;
#11675 = LINE ( 'NONE', #5920, #1760 ) ;
#11676 = CARTESIAN_POINT ( 'NONE',  ( -37.49999999999999289, -9.213203435596451385, -126.4213562373092685 ) ) ;
#11677 = CARTESIAN_POINT ( 'NONE',  ( -827.8090925714915329, 81.71768170412174470, -104.6809152895176851 ) ) ;
#11678 = CARTESIAN_POINT ( 'NONE',  ( -365.0000000000000568, 61.99999999999992895, -124.6807709998038405 ) ) ;
#11679 = CARTESIAN_POINT ( 'NONE',  ( 20.77382952161539720, 179.4090627415999961, -123.5337882278526251 ) ) ;
#11680 = ORIENTED_EDGE ( 'NONE', *, *, #2747, .F. ) ;
#11681 = DIRECTION ( 'NONE',  ( -1.000000000000000000, 0.000000000000000000, 0.000000000000000000 ) ) ;
#11682 = CARTESIAN_POINT ( 'NONE',  ( -951.4198147059589701, 125.0824040815807194, -124.6807709998040252 ) ) ;
#11683 = B_SPLINE_SURFACE_WITH_KNOTS ( 'NONE', 3, 3, ( 
 ( #8220, #9939, #2639, #11917, #12112, #2457, #6176, #12044, #1474, #3623, #11981, #10926, #3436, #5291, #10189, #1534, #6236, #5234, #9068, #1590 ),
 ( #668, #2516, #5415, #10122, #603, #1655, #11052, #6292, #732, #10002, #9005, #1729, #4378, #5487, #10061, #8151, #538, #3372, #4574, #10862 ),
 ( #9196, #8094, #3497, #7223, #9261, #5353, #4507, #803, #6417, #7286, #8287, #3555, #9129, #7162, #10989, #11117, #4443, #2397, #4320, #2577 ),
 ( #6349, #7345, #104, #5552, #8417, #9389, #12237, #2836, #928, #2028, #6481, #4701, #6603, #10367, #7531, #1908, #11187, #9568, #5785, #38 ),
 ( #8475, #1110, #7590, #3880, #10310, #5673, #3757, #2957, #868, #4638, #10255, #9506, #2709, #155, #4861, #3816, #12180, #3696, #8647, #1850 ),
 ( #11298, #7410, #7472, #985, #11252, #2777, #6662, #6540, #8526, #11361, #2898, #10495, #10432, #1975, #5731, #1051, #7651, #11421, #6720, #7709 ),
 ( #11485, #2151, #2330, #3018, #8873, #6779, #6962, #3074, #11727, #9623, #4069, #3129, #3242, #7022, #4003, #5850, #6846, #2269, #7836, #397 ),
 ( #6101, #8819, #11613, #9684, #9871, #4126, #1343, #10612, #6902, #5918, #10793, #1171, #4180, #4925, #10554, #2206, #8704, #5975, #9742, #6038 ),
 ( #2096, #219, #345, #7772, #1400, #10670, #5164, #8924, #3941, #1287, #11549, #3185, #1224, #4981, #8763, #7901, #11670, #282, #9804, #5041 ),
 ( #10731, #5106, #7959, #5469, #6280, #10050, #11787, #4492, #1518, #10175, #4309, #8020, #1641, #7083, #1710, #1581, #523, #5280, #7146, #12028 ),
 ( #8080, #10851, #10912, #3420, #454, #2503, #4367, #7269, #3484, #2442, #653, #10109, #3361, #10975, #6225, #8270, #2386, #717, #6158, #9924 ),
 ( #5342, #8992, #11101, #9989, #9116, #2625, #6403, #4430, #6336, #5219, #8206, #4249, #11849, #11036, #2565, #9055, #593, #8136, #11902, #5720 ),
 ( #2763, #10482, #11238, #3746, #11409, #4744, #9246, #4623, #4558, #12166, #6650, #8334, #3868, #2946, #91, #9436, #6709, #11170, #1775, #919 ),
 ( #2695, #788, #9311, #6467, #12221, #4688, #6527, #7455, #12098, #5537, #8462, #3607, #7398, #3680, #10296, #10240, #853, #11347, #8402, #2017 ),
 ( #1899, #1836, #5599, #7640, #9376, #8515, #7518, #11288, #2821, #6589, #10357, #5662, #28, #972, #3802, #7575, #2889, #10418, #1960, #9493 ),
 ( #1035, #4799, #8569, #5965, #9551, #6764, #1097, #3992, #4170, #4851, #10720, #8631, #8808, #4911, #1331, #11474, #5905, #4972, #5091, #8863 ),
 ( #7701, #8696, #4116, #9676, #2256, #9613, #6892, #5775, #146, #10781, #3230, #6028, #265, #3005, #3931, #5838, #10537, #8752, #1214, #11533 ),
 ( #2084, #1158, #4057, #207, #7760, #3062, #6831, #10600, #2140, #7888, #7824, #11598, #388, #10661, #3116, #2197, #7944, #9733, #5031, #1272 ),
 ( #329, #11657, #3176, #6952, #9791, #11717, #7009, #9909, #437, #5387, #10962, #506, #2490, #6266, #10037, #1567, #8183, #6086, #11021, #4227 ),
 ( #702, #10094, #1628, #9165, #4477, #12012, #10157, #1082, #7741, #4957, #10706, #2242, #11456, #9536, #2062, #8794, #11518, #313, #2988, #251 ),
 ( #2004, #378, #7627, #4101, #4040, #1142, #7873, #3164, #3044, #6694, #4893, #11395, #8617, #3914, #190, #6010, #425, #9086, #10824, #5252 ),
 ( #1494, #10022, #6995, #6193, #1552, #8171, #7180, #2413, #8111, #2365, #494, #7930, #625, #10765, #9898, #5374, #6131, #10879, #6313, #11874 ),
 ( #11764, #11704, #7052, #5316, #3219, #11009, #10081, #7243, #4341, #1612, #6071, #8898, #8053, #2301, #1434, #9150, #5192, #9961, #4157, #3390 ),
 ( #3277, #9836, #8964, #4397, #1375, #2538, #5138, #4215, #10950, #7993, #4283, #11820, #3339, #9024, #7117, #561, #2478, #6255, #11939, #3457 ),
 ( #11138, #4465, #5437, #12135, #3519, #7311, #3576, #10210, #10144, #12002, #2795, #8242, #5687, #7548, #5570, #1679, #9217, #11317, #7367, #12197 ),
 ( #10385, #11074, #1748, #756, #4533, #3715, #8309, #2600, #12066, #6372, #3775, #5510, #2665, #2732, #6439, #9285, #823, #887, #4596, #8370 ),
 ( #3648, #2858, #7427, #5633, #11207, #7492, #6500, #8491, #10274, #1808, #9345, #12239, #6622, #4658, #8434, #11266, #6563, #10328, #9407, #1869 ),
 ( #689, #943, #4715, #1926, #11261, #2724, #8303, #8428, #6494, #6433, #1605, #1672, #6306, #10074, #2532, #4526, #3641, #9211, #1862, #747 ),
 ( #4711, #5626, #5564, #12193, #9144, #9339, #3708, #9402, #8487, #684, #4457, #12058, #11131, #8236, #11996, #7303, #3570, #7362, #2659, #10203 ),
 ( #754, #2731, #2664, #59, #2794, #11686, #7792, #10510, #11500, #3957, #1305, #1127, #5806, #9522, #7725, #1188, #10451, #237, #2110, #5000 ),
 ( #3028, #9705, #5935, #5867, #302, #2044, #4824, #5058, #6798, #7919, #9643, #10571, #8600, #11438, #3205, #1989, #10689, #1244, #7669, #3095 ),
 ( #119, #6735, #1067, #5747, #4943, #3896, #4022, #8719, #4088, #7857, #11632, #9586, #3150, #2225, #5991, #9131, #7593, #4983, #2901, #6849 ),
 ( #7840, #5734, #158, #11487, #11615, #3133, #107, #9508, #5786, #2155, #3943, #8765, #3883, #4926, #41, #6663, #5044, #9744, #284, #8705 ),
 ( #1227, #4006, #7710, #1053, #9569, #3818, #4811, #8583, #3019, #2098, #7653, #4072, #9625, #220, #10671, #6906, #2208, #5976, #1289, #10854 ),
 ( #10052, #2388, #4183, #8084, #7024, #7904, #6964, #8995, #526, #3188, #7148, #11905, #10733, #2271, #3424, #5221, #7961, #6040, #1346, #11674 ),
 ( #9873, #9807, #6160, #10796, #5166, #1403, #4311, #347, #5109, #4128, #2332, #7210, #8876, #1521, #399, #11851, #11730, #8140, #3245, #8927 ) ),
 .UNSPECIFIED., .T., .F., .F.,
 ( 4, 1, 1, 1, 1, 1, 1, 1, 1, 1, 1, 1, 1, 1, 1, 1, 2, 1, 1, 1, 1, 1, 1, 1, 1, 1, 1, 1, 1, 1, 1, 1, 4 ),
 ( 4, 1, 1, 1, 2, 1, 1, 1, 2, 2, 2, 2, 4 ),
 ( 0.000000000000000000, 0.03125000000000000000, 0.06250000000000000000, 0.09375000000000000000, 0.1250000000000000000, 0.1562500000000000000, 0.1875000000000000000, 0.2187500000000000000, 0.2500000000000000000, 0.2812500000000000000, 0.3125000000000000000, 0.3437500000000000000, 0.3750000000000000000, 0.4062500000000000000, 0.4375000000000000000, 0.4687500000000000000, 0.5000000000000000000, 0.5312500000000000000, 0.5625000000000000000, 0.5937500000000000000, 0.6250000000000000000, 0.6562500000000000000, 0.6875000000000000000, 0.7187500000000000000, 0.7500000000000000000, 0.7812500000000000000, 0.8125000000000000000, 0.8437500000000000000, 0.8750000000000000000, 0.9062500000000000000, 0.9375000000000000000, 0.9687500000000000000, 1.000000000000000000 ),
 ( 0.000000000000000000, 0.04762575996673557022, 0.07143863995010346635, 0.09525151993347125146, 0.1428772799002068217, 0.1647615404280894369, 0.1757036706920307445, 0.1866458009559719411, 0.2085300614838545563, 0.4016963878702066726, 0.4307237013227157574, 0.6771470142487683308, 1.000000000000000000 ),
 .UNSPECIFIED. ) ;
#11684 = ADVANCED_FACE ( 'NONE', ( #3642 ), #7423, .T. ) ;
#11685 = CARTESIAN_POINT ( 'NONE',  ( 126.4213562373094959, -6.000000000000000000, -7.500000000000019540 ) ) ;
#11686 = CARTESIAN_POINT ( 'NONE',  ( -1031.329434936838197, 101.6864263019769083, -149.7857175106636305 ) ) ;
#11687 = AXIS2_PLACEMENT_3D ( 'NONE', #3320, #2224, #7976 ) ;
#11688 = ADVANCED_FACE ( 'NONE', ( #2725 ), #1606, .F. ) ;
#11689 = DIRECTION ( 'NONE',  ( -0.000000000000000000, -1.000000000000000000, -0.000000000000000000 ) ) ;
#11690 = VERTEX_POINT ( 'NONE', #11003 ) ;
#11691 = ORIENTED_EDGE ( 'NONE', *, *, #1998, .F. ) ;
#11692 = EDGE_CURVE ( 'NONE', #10573, #1414, #8304, .T. ) ;
#11693 = CARTESIAN_POINT ( 'NONE',  ( -379.2267265911639811, 62.10569044149951168, -127.0610581819159250 ) ) ;
#11694 = CARTESIAN_POINT ( 'NONE',  ( -853.6888141844391384, 53.84495383942815039, -152.5758913445293103 ) ) ;
#11695 = CARTESIAN_POINT ( 'NONE',  ( -820.5015944640223324, 74.92794535928011612, -143.3902763353424348 ) ) ;
#11696 = CIRCLE ( 'NONE', #10304, 7.500000000000007105 ) ;
#11697 = CARTESIAN_POINT ( 'NONE',  ( -374.7703100637729676, 87.70944966426152689, -153.9741766301830239 ) ) ;
#11698 = CARTESIAN_POINT ( 'NONE',  ( 2.187692937179487324E-12, 12.00000000000000000, 76.07864376269048989 ) ) ;
#11699 = CARTESIAN_POINT ( 'NONE',  ( -373.1928135428791506, 64.92830709045685467, -114.1675738471262633 ) ) ;
#11700 = CARTESIAN_POINT ( 'NONE',  ( -827.1370682460163835, 74.91132569719390233, -94.68188112044103377 ) ) ;
#11701 = CARTESIAN_POINT ( 'NONE',  ( -262.5000000000000000, 24.00000000000000711, -126.4213562373076059 ) ) ;
#11702 = DIRECTION ( 'NONE',  ( 0.000000000000000000, 1.000000000000000000, 0.000000000000000000 ) ) ;
#11703 = ORIENTED_EDGE ( 'NONE', *, *, #11161, .F. ) ;
#11704 = CARTESIAN_POINT ( 'NONE',  ( -1062.665377791219498, 57.01990411978283646, -146.0307792196448702 ) ) ;
#11705 = ADVANCED_FACE ( 'NONE', ( #1673 ), #6250, .F. ) ;
#11706 = AXIS2_PLACEMENT_3D ( 'NONE', #3611, #4627, #7580 ) ;
#11707 = ORIENTED_EDGE ( 'NONE', *, *, #3685, .F. ) ;
#11708 = EDGE_LOOP ( 'NONE', ( #10457, #4860 ) ) ;
#11709 = CARTESIAN_POINT ( 'NONE',  ( -997.4616017999825317, 44.34671234275855767, -107.9061927053325007 ) ) ;
#11710 = ORIENTED_EDGE ( 'NONE', *, *, #3820, .F. ) ;
#11711 = CARTESIAN_POINT ( 'NONE',  ( -828.6680473269018421, 79.97282626266093075, -94.86685776557048655 ) ) ;
#11712 = DIRECTION ( 'NONE',  ( -1.000000000000000000, 0.000000000000000000, 0.000000000000000000 ) ) ;
#11713 = ORIENTED_EDGE ( 'NONE', *, *, #7577, .T. ) ;
#11714 = CARTESIAN_POINT ( 'NONE',  ( -821.3231414384459868, 74.33484277641235849, -154.6590659353650494 ) ) ;
#11715 = ORIENTED_EDGE ( 'NONE', *, *, #1984, .T. ) ;
#11716 = ORIENTED_EDGE ( 'NONE', *, *, #2772, .F. ) ;
#11717 = CARTESIAN_POINT ( 'NONE',  ( -1032.658196452833636, 44.72920460984212809, -126.6442663926291914 ) ) ;
#11718 = DIRECTION ( 'NONE',  ( 1.000000000000000000, 0.000000000000000000, 0.000000000000000000 ) ) ;
#11719 = AXIS2_PLACEMENT_3D ( 'NONE', #1713, #8208, #10359 ) ;
#11720 = CARTESIAN_POINT ( 'NONE',  ( 0.000000000000000000, 7.794228634059941818, 4.500000000000007994 ) ) ;
#11721 = CARTESIAN_POINT ( 'NONE',  ( -1014.911393615048723, 99.73439156314999821, -96.78565065507932275 ) ) ;
#11722 = DIRECTION ( 'NONE',  ( -3.061276722312011504E-17, 1.000000000000000000, 0.000000000000000000 ) ) ;
#11723 = EDGE_LOOP ( 'NONE', ( #10250, #10882 ) ) ;
#11724 = CIRCLE ( 'NONE', #6981, 7.500000000000007105 ) ;
#11725 = SURFACE_STYLE_USAGE ( .BOTH. , #1169 ) ;
#11726 = ORIENTED_EDGE ( 'NONE', *, *, #3788, .F. ) ;
#11727 = CARTESIAN_POINT ( 'NONE',  ( -1018.692594135739682, 105.1726068785156656, -99.57582448894508786 ) ) ;
#11728 = DIRECTION ( 'NONE',  ( 0.000000000000000000, 1.000000000000000000, -0.000000000000000000 ) ) ;
#11729 = CARTESIAN_POINT ( 'NONE',  ( -974.1454360724337675, 123.6012932931491690, -130.5712005305403238 ) ) ;
#11730 = CARTESIAN_POINT ( 'NONE',  ( -904.2101318205999405, 125.2895275102983419, -124.6807709998041531 ) ) ;
#11731 = FACE_OUTER_BOUND ( 'NONE', #11210, .T. ) ;
#11732 = CYLINDRICAL_SURFACE ( 'NONE', #9706, 7.500000000000007105 ) ;
#11733 = AXIS2_PLACEMENT_3D ( 'NONE', #1754, #9413, #6505 ) ;
#11734 = ADVANCED_FACE ( 'NONE', ( #5432 ), #8237, .F. ) ;
#11735 = AXIS2_PLACEMENT_3D ( 'NONE', #10396, #4781, #1939 ) ;
#11736 = CARTESIAN_POINT ( 'NONE',  ( -1024.848917040348397, 116.4131098345821442, -113.1262384684097242 ) ) ;
#11737 = DIRECTION ( 'NONE',  ( 0.000000000000000000, 0.000000000000000000, 1.000000000000000000 ) ) ;
#11738 = CARTESIAN_POINT ( 'NONE',  ( -20.00000000000000000, 182.6968134406616002, -124.6807709998189466 ) ) ;
#11739 = EDGE_CURVE ( 'NONE', #7713, #9067, #9212, .T. ) ;
#11740 = CARTESIAN_POINT ( 'NONE',  ( -828.1711263241217011, 81.17408148015023528, -104.6959820179050951 ) ) ;
#11741 = CARTESIAN_POINT ( 'NONE',  ( -1021.637154595298057, 53.81063926482157456, -124.6807709998041958 ) ) ;
#11742 = CARTESIAN_POINT ( 'NONE',  ( 21.02894813693603382, 178.6886507591858049, -125.1318251072521832 ) ) ;
#11743 = ORIENTED_EDGE ( 'NONE', *, *, #5405, .F. ) ;
#11744 = DIRECTION ( 'NONE',  ( 0.000000000000000000, -1.000000000000000000, -7.930164461608263644E-17 ) ) ;
#11745 = CARTESIAN_POINT ( 'NONE',  ( 7.500000000000000000, -5.196152422706638241, -9.000000000000001776 ) ) ;
#11746 = EDGE_CURVE ( 'NONE', #5383, #725, #2041, .T. ) ;
#11747 = AXIS2_PLACEMENT_3D ( 'NONE', #10058, #11184, #12040 ) ;
#11748 = AXIS2_PLACEMENT_3D ( 'NONE', #7750, #7511, #2813 ) ;
#11749 = LINE ( 'NONE', #8888, #4177 ) ;
#11750 = CARTESIAN_POINT ( 'NONE',  ( 21.06240745282767435, 180.2041921146315246, -126.4269926335259413 ) ) ;
#11751 = EDGE_LOOP ( 'NONE', ( #5022, #8743, #5083, #9349 ) ) ;
#11752 = CARTESIAN_POINT ( 'NONE',  ( 19.95943535220619580, 180.3310120364355953, -123.1936495657158019 ) ) ;
#11753 = CIRCLE ( 'NONE', #5416, 7.500000000000007105 ) ;
#11754 = AXIS2_PLACEMENT_3D ( 'NONE', #8835, #6920, #7793 ) ;
#11755 = EDGE_CURVE ( 'NONE', #192, #5774, #10756, .T. ) ;
#11756 = FACE_BOUND ( 'NONE', #12042, .T. ) ;
#11757 = CARTESIAN_POINT ( 'NONE',  ( -819.2376510598713821, 55.50059629688480811, -152.5758913445292535 ) ) ;
#11758 = ADVANCED_FACE ( 'NONE', ( #2968 ), #5800, .F. ) ;
#11759 = CARTESIAN_POINT ( 'NONE',  ( -372.3000261716298382, 101.2597060943377301, -145.0788949275182347 ) ) ;
#11760 = CARTESIAN_POINT ( 'NONE',  ( -27.99999999999999645, -6.000000000000000000, -27.99999999999999645 ) ) ;
#11761 = CARTESIAN_POINT ( 'NONE',  ( -371.0605248364101953, 58.84368270872280249, -110.5171750812754965 ) ) ;
#11762 = FACE_OUTER_BOUND ( 'NONE', #3528, .T. ) ;
#11763 = VERTEX_POINT ( 'NONE', #10569 ) ;
#11764 = CARTESIAN_POINT ( 'NONE',  ( -1065.000000000007731, 60.65002596136951496, -146.0307792196448986 ) ) ;
#11765 = AXIS2_PLACEMENT_3D ( 'NONE', #470, #11799, #4265 ) ;
#11766 = ORIENTED_EDGE ( 'NONE', *, *, #403, .T. ) ;
#11767 = CARTESIAN_POINT ( 'NONE',  ( 6.899999999999999467, 10.39230484541326938, 0.000000000000000000 ) ) ;
#11768 = CARTESIAN_POINT ( 'NONE',  ( -1021.483947769352199, 56.15424078096101113, -113.1262384684096105 ) ) ;
#11769 = EDGE_CURVE ( 'NONE', #2477, #502, #4257, .T. ) ;
#11770 = CARTESIAN_POINT ( 'NONE',  ( -826.0438798663770967, 83.15978422364159428, -95.19800250875974257 ) ) ;
#11771 = CARTESIAN_POINT ( 'NONE',  ( 7.500000000000006217, 197.0000000000000000, -124.6807709998038405 ) ) ;
#11772 = ORIENTED_EDGE ( 'NONE', *, *, #4565, .F. ) ;
#11773 = B_SPLINE_CURVE_WITH_KNOTS ( 'NONE', 3,
 ( #11177, #922, #3490, #4695, #12231, #658, #11043, #12034, #6340, #10115, #3750, #3547, #11108, #2769, #7523, #3612, #2630, #6285, #9251, #861, #5346, #10180, #1717, #4562, #5476, #794, #8339, #4629, #12103, #8409, #12171, #7464, #3688, #3012, #3997, #6593 ),
 .UNSPECIFIED., .F., .F.,
 ( 4, 2, 2, 2, 2, 2, 2, 2, 2, 2, 2, 2, 2, 2, 2, 2, 2, 4 ),
 ( 0.01566607101767040003, 0.01666400919013317009, 0.01766194736259593667, 0.01865988553505870673, 0.01965782370752147332, 0.02065576187998424337, 0.02165370005244700996, 0.02215266913867839152, 0.02265163822490976961, 0.02364957639737220313, 0.02464751456983464012, 0.02564545274229707017, 0.02664339091475950369, 0.02764132908722193721, 0.02863926725968437073, 0.02963720543214680425, 0.03063514360460923777, 0.03163308177707167129 ),
 .UNSPECIFIED. ) ;
#11774 = ORIENTED_EDGE ( 'NONE', *, *, #2675, .T. ) ;
#11775 = CARTESIAN_POINT ( 'NONE',  ( 0.000000000000000000, 0.000000000000000000, 0.000000000000000000 ) ) ;
#11776 = CARTESIAN_POINT ( 'NONE',  ( -210.0000000000000000, 12.00000000000001421, -126.4213562373080180 ) ) ;
#11777 = DIRECTION ( 'NONE',  ( -1.000000000000000000, 0.000000000000000000, 0.000000000000000000 ) ) ;
#11778 = AXIS2_PLACEMENT_3D ( 'NONE', #2875, #3049, #77 ) ;
#11779 = B_SPLINE_CURVE_WITH_KNOTS ( 'NONE', 3,
 ( #11098, #6645, #9432, #8511, #5715, #1771, #5658, #11284, #3677, #4740, #11340, #5531, #2688, #1029, #9306, #2759, #8330, #6461, #21, #7392, #7331, #4683, #2621, #10413, #6523, #1956, #2883, #9488, #1832, #4618, #3798, #8396, #6398, #10169, #7448, #5595, #12022, #9371 ),
 .UNSPECIFIED., .F., .F.,
 ( 4, 2, 2, 2, 2, 2, 2, 2, 2, 2, 2, 2, 2, 2, 2, 2, 2, 2, 4 ),
 ( 0.01596000347429163760, 0.01693787742768196672, 0.01791575138107229584, 0.01840468835776752285, 0.01889362533446274986, 0.01987149928785320388, 0.02084937324124365790, 0.02182724719463410845, 0.02280512114802456247, 0.02378299510141501649, 0.02476086905480547051, 0.02573874300819592453, 0.02671661696158637855, 0.02720555393828160556, 0.02769449091497682910, 0.02867236486836731088, 0.02965023882175778919, 0.03062811277514827096, 0.03160598672853875274 ),
 .UNSPECIFIED. ) ;
#11780 = CARTESIAN_POINT ( 'NONE',  ( -853.2189900670988436, 91.12674563889150647, -96.78565065507912379 ) ) ;
#11781 = LINE ( 'NONE', #10900, #3174 ) ;
#11782 = VERTEX_POINT ( 'NONE', #3709 ) ;
#11783 = ORIENTED_EDGE ( 'NONE', *, *, #7123, .T. ) ;
#11784 = DIRECTION ( 'NONE',  ( 0.3117078928809249860, -1.670400663243698742E-14, 0.9501779778103330854 ) ) ;
#11785 = ORIENTED_EDGE ( 'NONE', *, *, #10410, .T. ) ;
#11786 = CARTESIAN_POINT ( 'NONE',  ( 0.000000000000000000, 0.000000000000000000, 0.000000000000000000 ) ) ;
#11787 = CARTESIAN_POINT ( 'NONE',  ( -1026.651933061283898, 84.71212313386838844, -94.48732055948616448 ) ) ;
#11788 = AXIS2_PLACEMENT_3D ( 'NONE', #10421, #7459, #7520 ) ;
#11789 = FACE_OUTER_BOUND ( 'NONE', #3900, .T. ) ;
#11790 = CARTESIAN_POINT ( 'NONE',  ( -21.02406183884818347, 181.6953053563225353, -125.1140174421107929 ) ) ;
#11791 = DIRECTION ( 'NONE',  ( -1.000000000000000000, -0.000000000000000000, -6.195440985631455317E-17 ) ) ;
#11792 = DIRECTION ( 'NONE',  ( -8.163404592832030268E-17, 1.000000000000000000, -0.000000000000000000 ) ) ;
#11793 = CIRCLE ( 'NONE', #1525, 7.500000000000007105 ) ;
#11794 = DIRECTION ( 'NONE',  ( 1.186840563529527301E-16, -1.000000000000000000, 0.000000000000000000 ) ) ;
#11795 = AXIS2_PLACEMENT_3D ( 'NONE', #6210, #774, #642 ) ;
#11796 = FACE_BOUND ( 'NONE', #6265, .T. ) ;
#11797 = CARTESIAN_POINT ( 'NONE',  ( -22.49999999999997868, 24.00000000000001421, -126.4213562373092685 ) ) ;
#11798 = CARTESIAN_POINT ( 'NONE',  ( -819.1470717756643580, 80.43796722965394963, -94.85155950616754694 ) ) ;
#11799 = DIRECTION ( 'NONE',  ( 0.000000000000000000, 0.000000000000000000, -1.000000000000000000 ) ) ;
#11800 = ORIENTED_EDGE ( 'NONE', *, *, #2610, .F. ) ;
#11801 = CARTESIAN_POINT ( 'NONE',  ( -925.0000000000000000, 101.9999999999999858, -124.6807709998038405 ) ) ;
#11802 = CARTESIAN_POINT ( 'NONE',  ( -795.0000000000047748, 112.0000000000007532, -124.6807709998042384 ) ) ;
#11803 = EDGE_CURVE ( 'NONE', #7797, #11532, #8408, .T. ) ;
#11804 = DIRECTION ( 'NONE',  ( -8.163404592832030268E-17, 1.000000000000000000, -0.000000000000000000 ) ) ;
#11805 = DIRECTION ( 'NONE',  ( 0.000000000000000000, 0.000000000000000000, 1.000000000000000000 ) ) ;
#11806 = DIRECTION ( 'NONE',  ( -0.000000000000000000, -0.000000000000000000, -1.000000000000000000 ) ) ;
#11807 = ORIENTED_EDGE ( 'NONE', *, *, #6967, .T. ) ;
#11808 = VERTEX_POINT ( 'NONE', #9403 ) ;
#11809 = CARTESIAN_POINT ( 'NONE',  ( 20.73848121498308572, 179.7277624624672399, -123.3832113358915876 ) ) ;
#11810 = AXIS2_PLACEMENT_3D ( 'NONE', #4625, #8207, #4431 ) ;
#11811 = CARTESIAN_POINT ( 'NONE',  ( -382.5120035867337265, 68.79460237993339433, -139.7124243609125642 ) ) ;
#11812 = CARTESIAN_POINT ( 'NONE',  ( -1056.430032577873362, 71.19035303699479300, -154.2940595301283793 ) ) ;
#11813 = CARTESIAN_POINT ( 'NONE',  ( -821.1548363108421427, 74.44610204637938011, -143.1996371447164904 ) ) ;
#11814 = CIRCLE ( 'NONE', #760, 7.500000000000012434 ) ;
#11815 = CARTESIAN_POINT ( 'NONE',  ( -371.4259950879257985, 104.0958151038622646, -140.9456086550797238 ) ) ;
#11816 = CARTESIAN_POINT ( 'NONE',  ( 0.000000000000000000, 0.000000000000000000, 9.000000000000000000 ) ) ;
#11817 = CARTESIAN_POINT ( 'NONE',  ( -373.6571679095217746, 67.00567956805471681, -111.2964104634416174 ) ) ;
#11818 = LINE ( 'NONE', #3333, #8851 ) ;
#11819 = VERTEX_POINT ( 'NONE', #3771 ) ;
#11820 = CARTESIAN_POINT ( 'NONE',  ( -996.5513353153702383, 56.29506814688406990, -149.7857175106634600 ) ) ;
#11821 = EDGE_CURVE ( 'NONE', #7471, #10331, #7809, .T. ) ;
#11822 = APPLICATION_CONTEXT ( 'automotive_design' ) ;
#11823 = CIRCLE ( 'NONE', #7283, 7.500000000000007105 ) ;
#11824 = ORIENTED_EDGE ( 'NONE', *, *, #7451, .F. ) ;
#11825 = ADVANCED_FACE ( 'NONE', ( #7608 ), #11373, .T. ) ;
#11826 = CARTESIAN_POINT ( 'NONE',  ( 6.899999999999999467, 5.196152422706624918, 8.999999999999998224 ) ) ;
#11827 = CARTESIAN_POINT ( 'NONE',  ( -27.99999999999999645, -492.9999999999998863, -27.99999999999999645 ) ) ;
#11828 = ORIENTED_EDGE ( 'NONE', *, *, #10225, .T. ) ;
#11829 = CARTESIAN_POINT ( 'NONE',  ( -827.8052707278029629, 81.72255078513846627, -95.02959508169305991 ) ) ;
#11830 = MECHANICAL_DESIGN_GEOMETRIC_PRESENTATION_REPRESENTATION (  '', ( #3324 ), #2162 ) ;
#11831 = CARTESIAN_POINT ( 'NONE',  ( -270.0000000000000000, 139.9999999999999716, -126.4213562373076059 ) ) ;
#11832 = ORIENTED_EDGE ( 'NONE', *, *, #3485, .T. ) ;
#11833 = CARTESIAN_POINT ( 'NONE',  ( -141.4213562373095101, -6.000000000000000000, 3.644282033693712520E-14 ) ) ;
#11834 = ORIENTED_EDGE ( 'NONE', *, *, #11843, .T. ) ;
#11835 = ADVANCED_FACE ( 'NONE', ( #297, #4082, #232, #8831, #5052, #4142, #4018, #7973, #3256, #2281, #7097 ), #5986, .F. ) ;
#11836 = DIRECTION ( 'NONE',  ( -0.000000000000000000, 1.000000000000000000, -0.000000000000000000 ) ) ;
#11837 = EDGE_CURVE ( 'NONE', #3207, #10717, #6032, .T. ) ;
#11838 = EDGE_CURVE ( 'NONE', #2536, #7974, #10766, .T. ) ;
#11839 = AXIS2_PLACEMENT_3D ( 'NONE', #9316, #1841, #10301 ) ;
#11840 = CARTESIAN_POINT ( 'NONE',  ( -903.6727718956999524, 110.0506089609176712, -99.57582448894470417 ) ) ;
#11841 = DIRECTION ( 'NONE',  ( 1.000000000000000000, 0.000000000000000000, -0.000000000000000000 ) ) ;
#11842 = EDGE_CURVE ( 'NONE', #9384, #2309, #6914, .T. ) ;
#11843 = EDGE_CURVE ( 'NONE', #3288, #3585, #483, .T. ) ;
#11844 = ORIENTED_EDGE ( 'NONE', *, *, #11692, .F. ) ;
#11845 = CARTESIAN_POINT ( 'NONE',  ( -21.06817635203014305, 179.2720927603041332, -126.1063812806455218 ) ) ;
#11846 = LINE ( 'NONE', #715, #8009 ) ;
#11847 = ORIENTED_EDGE ( 'NONE', *, *, #9644, .T. ) ;
#11848 = CARTESIAN_POINT ( 'NONE',  ( -828.1698196941869128, 81.17660424754099324, -154.3879017162145146 ) ) ;
#11849 = CARTESIAN_POINT ( 'NONE',  ( -975.5821371384171243, 62.83201726680821508, -96.78565065507949328 ) ) ;
#11850 = DIRECTION ( 'NONE',  ( -1.000000000000000000, 0.000000000000000000, 0.000000000000000000 ) ) ;
#11851 = CARTESIAN_POINT ( 'NONE',  ( -926.5138833012647410, 125.7648744980332225, -124.6807709998040394 ) ) ;
#11852 = EDGE_CURVE ( 'NONE', #3787, #8948, #9973, .T. ) ;
#11853 = DIRECTION ( 'NONE',  ( 3.061276722312011504E-17, -1.000000000000000000, 0.000000000000000000 ) ) ;
#11854 = CARTESIAN_POINT ( 'NONE',  ( -45.53315400109751465, 12.00000000000000000, -230.3419396193594366 ) ) ;
#11855 = CARTESIAN_POINT ( 'NONE',  ( -825.1278902672576123, 83.51360356663558093, -104.7380248171173918 ) ) ;
#11856 = CARTESIAN_POINT ( 'NONE',  ( -379.1756773959688189, 62.02252057344967540, -123.5830889625225240 ) ) ;
#11857 = ORIENTED_EDGE ( 'NONE', *, *, #7658, .F. ) ;
#11858 = CARTESIAN_POINT ( 'NONE',  ( -379.7921418149325063, 63.07164944986214294, -118.2218589047913611 ) ) ;
#11859 = DIRECTION ( 'NONE',  ( 3.061276722312011504E-17, -1.000000000000000000, 0.000000000000000000 ) ) ;
#11860 = FACE_OUTER_BOUND ( 'NONE', #7344, .T. ) ;
#11861 = CARTESIAN_POINT ( 'NONE',  ( -372.5553489903112450, 63.65594039108665925, -103.2085620308231313 ) ) ;
#11862 = LINE ( 'NONE', #9763, #4602 ) ;
#11863 = EDGE_LOOP ( 'NONE', ( #11924, #10079 ) ) ;
#11864 = CARTESIAN_POINT ( 'NONE',  ( -19.91081574664456610, 181.5182364730087272, -122.7941294590837913 ) ) ;
#11865 = FACE_OUTER_BOUND ( 'NONE', #1482, .T. ) ;
#11866 = CARTESIAN_POINT ( 'NONE',  ( -372.5444667781683847, 101.5648799869878616, -129.1176400678176890 ) ) ;
#11867 = DIRECTION ( 'NONE',  ( 0.000000000000000000, 1.000000000000000000, 0.000000000000000000 ) ) ;
#11868 = CARTESIAN_POINT ( 'NONE',  ( 1.875296586882326249E-12, -6.000000000000004441, 46.07864376269049700 ) ) ;
#11869 = FACE_OUTER_BOUND ( 'NONE', #10103, .T. ) ;
#11870 = CARTESIAN_POINT ( 'NONE',  ( -824.1630149179034106, 73.67461580146778033, -94.71311452716244617 ) ) ;
#11871 = AXIS2_PLACEMENT_3D ( 'NONE', #9821, #9940, #10750 ) ;
#11872 = SURFACE_STYLE_USAGE ( .BOTH. , #3516 ) ;
#11873 = ORIENTED_EDGE ( 'NONE', *, *, #10249, .T. ) ;
#11874 = CARTESIAN_POINT ( 'NONE',  ( -795.0000000000002274, 56.89504896194490868, -141.4553492942756350 ) ) ;
#11875 = ORIENTED_EDGE ( 'NONE', *, *, #9166, .T. ) ;
#11876 = ORIENTED_EDGE ( 'NONE', *, *, #7214, .F. ) ;
#11877 = DIRECTION ( 'NONE',  ( -0.000000000000000000, 1.000000000000000000, -0.000000000000000000 ) ) ;
#11878 = AXIS2_PLACEMENT_3D ( 'NONE', #9646, #5689, #1128 ) ;
#11879 = EDGE_CURVE ( 'NONE', #2829, #6938, #11562, .T. ) ;
#11880 = CARTESIAN_POINT ( 'NONE',  ( -19.84982438750066081, 181.1124051037951119, -127.1282150172683458 ) ) ;
#11881 = ADVANCED_FACE ( 'NONE', ( #407 ), #4195, .F. ) ;
#11882 = ORIENTED_EDGE ( 'NONE', *, *, #4181, .F. ) ;
#11883 = DIRECTION ( 'NONE',  ( 0.000000000000000000, 0.000000000000000000, 1.000000000000000000 ) ) ;
#11884 = CARTESIAN_POINT ( 'NONE',  ( -379.2287960991276350, 101.8908318547082956, -122.2816696692770790 ) ) ;
#11885 = ORIENTED_EDGE ( 'NONE', *, *, #5656, .T. ) ;
#11886 = VERTEX_POINT ( 'NONE', #8033 ) ;
#11887 = CIRCLE ( 'NONE', #5970, 7.500000000000007994 ) ;
#11888 = EDGE_CURVE ( 'NONE', #9215, #10168, #9697, .T. ) ;
#11889 = CARTESIAN_POINT ( 'NONE',  ( 35.00000000000000000, 81.99999999999998579, 260.3192290001960032 ) ) ;
#11890 = CARTESIAN_POINT ( 'NONE',  ( 0.5584673446549119902, 5.621163452808791483, 8.263859302085860392 ) ) ;
#11891 = CARTESIAN_POINT ( 'NONE',  ( -975.1903095749676140, 79.73237568579435219, -94.48732055948607922 ) ) ;
#11892 = DIRECTION ( 'NONE',  ( -0.7071067811865479058, 0.000000000000000000, -0.7071067811865472397 ) ) ;
#11893 = DIRECTION ( 'NONE',  ( 0.000000000000000000, 0.000000000000000000, 1.000000000000000000 ) ) ;
#11894 = AXIS2_PLACEMENT_3D ( 'NONE', #900, #4668, #8446 ) ;
#11895 = EDGE_LOOP ( 'NONE', ( #7639, #971, #9920, #5290 ) ) ;
#11896 = PLANE ( 'NONE',  #11545 ) ;
#11897 = EDGE_CURVE ( 'NONE', #3398, #2733, #11627, .T. ) ;
#11898 =( NAMED_UNIT ( * ) PLANE_ANGLE_UNIT ( ) SI_UNIT ( $, .RADIAN. ) );
#11899 = DIRECTION ( 'NONE',  ( -0.000000000000000000, 1.000000000000000000, -0.000000000000000000 ) ) ;
#11900 = ORIENTED_EDGE ( 'NONE', *, *, #3742, .T. ) ;
#11901 = CARTESIAN_POINT ( 'NONE',  ( -828.3244535745621988, 80.88628718089528036, -154.4158655367039330 ) ) ;
#11902 = CARTESIAN_POINT ( 'NONE',  ( -819.2376510598700179, 55.50059629688461627, -96.78565065507937959 ) ) ;
#11903 = LINE ( 'NONE', #8403, #6681 ) ;
#11904 = CYLINDRICAL_SURFACE ( 'NONE', #1725, 7.500000000000013323 ) ;
#11905 = CARTESIAN_POINT ( 'NONE',  ( -991.5701548301635739, 122.8678427087061493, -126.6442663926292056 ) ) ;
#11906 = MANIFOLD_SOLID_BREP ( 'HeadFillet', #10834 ) ;
#11907 = PRODUCT_RELATED_PRODUCT_CATEGORY ( 'part', '', ( #4767 ) ) ;
#11908 = EDGE_LOOP ( 'NONE', ( #7574, #9297 ) ) ;
#11909 = CARTESIAN_POINT ( 'NONE',  ( -828.7881391348988700, 78.01879388416006122, -144.2812265043193349 ) ) ;
#11910 = AXIS2_PLACEMENT_3D ( 'NONE', #3764, #3948, #11429 ) ;
#11911 = DIRECTION ( 'NONE',  ( 0.000000000000000000, -1.000000000000000000, -7.930164461608263644E-17 ) ) ;
#11912 = CARTESIAN_POINT ( 'NONE',  ( -998.0431609429220998, 37.14019503514176535, -124.6807709998042668 ) ) ;
#11913 = CARTESIAN_POINT ( 'NONE',  ( -818.8285638327253082, 78.34424586195346762, -154.6388909787697798 ) ) ;
#11914 = EDGE_CURVE ( 'NONE', #4463, #647, #11948, .T. ) ;
#11915 = VERTEX_POINT ( 'NONE', #1454 ) ;
#11916 = CARTESIAN_POINT ( 'NONE',  ( -30.00000000000000000, -492.9999999999998863, 30.00000000000000000 ) ) ;
#11917 = CARTESIAN_POINT ( 'NONE',  ( -1045.864486809339724, 115.5688325305733741, -124.6807709998043663 ) ) ;
#11918 = DIRECTION ( 'NONE',  ( -0.7071067811865473507, 0.000000000000000000, 0.7071067811865477948 ) ) ;
#11919 = CARTESIAN_POINT ( 'NONE',  ( 3.123963502971610252E-13, 0.000000000000000000, -88.92135623730948168 ) ) ;
#11920 = DIRECTION ( 'NONE',  ( -8.163404592832030268E-17, 1.000000000000000000, -0.000000000000000000 ) ) ;
#11921 = VECTOR ( 'NONE', #723, 1000.000000000000000 ) ;
#11922 = AXIS2_PLACEMENT_3D ( 'NONE', #8846, #8790, #4154 ) ;
#11923 = CARTESIAN_POINT ( 'NONE',  ( 20.97617298093462779, 181.6955223378353992, -124.6801735093379477 ) ) ;
#11924 = ORIENTED_EDGE ( 'NONE', *, *, #12205, .T. ) ;
#11925 = CARTESIAN_POINT ( 'NONE',  ( -1065.000000000006594, 112.0000000000007105, -124.6807709998041531 ) ) ;
#11926 = CARTESIAN_POINT ( 'NONE',  ( -19.88356468709224956, 179.4771400433740780, -122.5253713362719594 ) ) ;
#11927 = CARTESIAN_POINT ( 'NONE',  ( -202.4999999999999716, 24.00000000000000711, -126.4213562373080180 ) ) ;
#11928 = DIRECTION ( 'NONE',  ( -0.000000000000000000, -1.000000000000000000, -0.000000000000000000 ) ) ;
#11929 = VECTOR ( 'NONE', #11259, 999.9999999999998863 ) ;
#11930 = VECTOR ( 'NONE', #996, 1000.000000000000000 ) ;
#11931 = CARTESIAN_POINT ( 'NONE',  ( 0.3563104543936312929, -9.539178283403842329, 1.477658550686872907 ) ) ;
#11932 = CYLINDRICAL_SURFACE ( 'NONE', #9563, 7.500000000000007105 ) ;
#11933 = AXIS2_PLACEMENT_3D ( 'NONE', #10968, #6273, #12158 ) ;
#11934 = DIRECTION ( 'NONE',  ( -1.000000000000000000, -0.000000000000000000, 0.000000000000000000 ) ) ;
#11935 = ORIENTED_EDGE ( 'NONE', *, *, #5319, .T. ) ;
#11936 = DIRECTION ( 'NONE',  ( -1.186840563529527301E-16, 1.000000000000000000, -0.000000000000000000 ) ) ;
#11937 = EDGE_CURVE ( 'NONE', #2064, #759, #9589, .T. ) ;
#11938 = EDGE_LOOP ( 'NONE', ( #2856, #379, #2220, #9803, #1318, #9897 ) ) ;
#11939 = CARTESIAN_POINT ( 'NONE',  ( -818.6751755801125228, 47.70925804672287995, -149.7857175106634884 ) ) ;
#11940 = ORIENTED_EDGE ( 'NONE', *, *, #5993, .F. ) ;
#11941 = VECTOR ( 'NONE', #10283, 1000.000000000000000 ) ;
#11942 = EDGE_LOOP ( 'NONE', ( #6968, #3864, #6661, #10323 ) ) ;
#11943 = CARTESIAN_POINT ( 'NONE',  ( -19.86685153722994457, 181.4191362699532704, -126.9922420271958288 ) ) ;
#11944 = EDGE_LOOP ( 'NONE', ( #7617, #8544, #3575, #4590 ) ) ;
#11945 = CARTESIAN_POINT ( 'NONE',  ( -372.4795512858445932, 62.20687173184607843, -127.6666720957034613 ) ) ;
#11946 = CARTESIAN_POINT ( 'NONE',  ( 126.4213562373094959, -6.000000000000000000, -6.938893903907228378E-15 ) ) ;
#11947 = VERTEX_POINT ( 'NONE', #3417 ) ;
#11948 = CIRCLE ( 'NONE', #1691, 7.500000000000007105 ) ;
#11949 = VERTEX_POINT ( 'NONE', #5216 ) ;
#11950 = ADVANCED_FACE ( 'NONE', ( #5338 ), #3304, .F. ) ;
#11951 = CYLINDRICAL_SURFACE ( 'NONE', #3853, 5.000000000000115463 ) ;
#11952 = CARTESIAN_POINT ( 'NONE',  ( 0.000000000000000000, 0.000000000000000000, 0.000000000000000000 ) ) ;
#11953 = DIRECTION ( 'NONE',  ( 0.000000000000000000, 0.000000000000000000, 1.000000000000000000 ) ) ;
#11954 = EDGE_CURVE ( 'NONE', #9851, #559, #1299, .T. ) ;
#11955 = LINE ( 'NONE', #7441, #133 ) ;
#11956 = CARTESIAN_POINT ( 'NONE',  ( -818.9903241194234624, 79.97817460710089676, -154.5468534023889049 ) ) ;
#11957 = AXIS2_PLACEMENT_3D ( 'NONE', #9048, #10904, #7955 ) ;
#11958 = CARTESIAN_POINT ( 'NONE',  ( -1015.825132819593136, 80.44428838836749662, -95.06748246948035330 ) ) ;
#11959 = CARTESIAN_POINT ( 'NONE',  ( 1.874378101782966050E-12, 152.0000000000000000, 61.07864376269052542 ) ) ;
#11960 = DIRECTION ( 'NONE',  ( 0.000000000000000000, 1.000000000000000000, 0.000000000000000000 ) ) ;
#11961 = CARTESIAN_POINT ( 'NONE',  ( -142.5000000000000000, 152.0000000000000000, -126.4213562373084301 ) ) ;
#11962 = DIRECTION ( 'NONE',  ( 0.000000000000000000, 0.000000000000000000, 1.000000000000000000 ) ) ;
#11963 = ORIENTED_EDGE ( 'NONE', *, *, #7191, .T. ) ;
#11964 = CARTESIAN_POINT ( 'NONE',  ( -822.0656543776474336, 83.35610039114051517, -154.1646031964236556 ) ) ;
#11965 = LINE ( 'NONE', #2627, #10814 ) ;
#11966 = FACE_BOUND ( 'NONE', #7006, .T. ) ;
#11967 = CARTESIAN_POINT ( 'NONE',  ( 6.257111856936825515E-13, 12.00000000000000000, -73.92135623730949590 ) ) ;
#11968 = DIRECTION ( 'NONE',  ( 0.7071067811865479058, 0.000000000000000000, 0.7071067811865472397 ) ) ;
#11969 = EDGE_CURVE ( 'NONE', #7745, #11140, #8209, .T. ) ;
#11970 = CIRCLE ( 'NONE', #9204, 0.9999999999999991118 ) ;
#11971 = EDGE_CURVE ( 'NONE', #2282, #6215, #6815, .T. ) ;
#11972 = DIRECTION ( 'NONE',  ( -0.000000000000000000, 1.000000000000000000, 0.000000000000000000 ) ) ;
#11973 = CARTESIAN_POINT ( 'NONE',  ( -19.90421694283016407, 179.0016913079787173, -122.7245617132216040 ) ) ;
#11974 = CARTESIAN_POINT ( 'NONE',  ( -821.5848584200502955, 74.20299736547755742, -143.0985335409774564 ) ) ;
#11975 = ORIENTED_EDGE ( 'NONE', *, *, #12081, .F. ) ;
#11976 = CARTESIAN_POINT ( 'NONE',  ( -370.3216402360161510, 56.83652478535064034, -116.0642080048412765 ) ) ;
#11977 = CONTEXT_DEPENDENT_SHAPE_REPRESENTATION ( #6924, #7832 ) ;
#11978 = AXIS2_PLACEMENT_3D ( 'NONE', #3745, #7397, #4687 ) ;
#11979 = ORIENTED_EDGE ( 'NONE', *, *, #8508, .F. ) ;
#11980 = CARTESIAN_POINT ( 'NONE',  ( 0.000000000000000000, 7.794228634059941818, 4.500000000000007994 ) ) ;
#11981 = CARTESIAN_POINT ( 'NONE',  ( -1010.922847972425529, 120.6260792194948550, -124.6807709998039542 ) ) ;
#11982 = CARTESIAN_POINT ( 'NONE',  ( -141.4213562373095101, -494.9999999999998863, 3.644282033693712520E-14 ) ) ;
#11983 = CARTESIAN_POINT ( 'NONE',  ( 6.899999999999999467, 0.000000000000000000, 0.000000000000000000 ) ) ;
#11984 = CARTESIAN_POINT ( 'NONE',  ( -371.5518914047726753, 60.29737756751269728, -107.7881083410018590 ) ) ;
#11985 = CARTESIAN_POINT ( 'NONE',  ( 19.99429366071382930, 181.6100965659588553, -125.2310411471055716 ) ) ;
#11986 = EDGE_CURVE ( 'NONE', #5042, #2268, #11846, .T. ) ;
#11987 = ORIENTED_EDGE ( 'NONE', *, *, #2285, .F. ) ;
#11988 = EDGE_CURVE ( 'NONE', #8074, #8885, #1578, .T. ) ;
#11989 = VERTEX_POINT ( 'NONE', #7206 ) ;
#11990 = DIRECTION ( 'NONE',  ( 1.000000000000000000, 0.000000000000000000, -0.000000000000000000 ) ) ;
#11991 = DIRECTION ( 'NONE',  ( -0.000000000000000000, 1.000000000000000000, -0.000000000000000000 ) ) ;
#11992 = CARTESIAN_POINT ( 'NONE',  ( -903.2629211055218548, 97.63080833215174437, -154.2940595301276971 ) ) ;
#11993 = CARTESIAN_POINT ( 'NONE',  ( -372.7918232332913817, 100.6587063813212524, -131.9323245634151647 ) ) ;
#11994 = CARTESIAN_POINT ( 'NONE',  ( 126.4213562373094959, 0.000000000000000000, -6.938893903907228378E-15 ) ) ;
#11995 = DIRECTION ( 'NONE',  ( 0.000000000000000000, 1.000000000000000000, 6.938893903907169213E-16 ) ) ;
#11996 = CARTESIAN_POINT ( 'NONE',  ( -952.4132309232853686, 101.5728619241206161, -152.5758913445289409 ) ) ;
#11997 = FACE_OUTER_BOUND ( 'NONE', #753, .T. ) ;
#11998 = VERTEX_POINT ( 'NONE', #9986 ) ;
#11999 = DIRECTION ( 'NONE',  ( -8.163404592832030268E-17, 1.000000000000000000, -0.000000000000000000 ) ) ;
#12000 = AXIS2_PLACEMENT_3D ( 'NONE', #10399, #8449, #10341 ) ;
#12001 = VERTEX_POINT ( 'NONE', #6333 ) ;
#12002 = CARTESIAN_POINT ( 'NONE',  ( -1016.123300349502756, 74.17810748283176281, -152.5758913445294525 ) ) ;
#12003 = ORIENTED_EDGE ( 'NONE', *, *, #238, .F. ) ;
#12004 = AXIS2_PLACEMENT_3D ( 'NONE', #1431, #9896, #3388 ) ;
#12005 = CARTESIAN_POINT ( 'NONE',  ( 7.750278301654327992E-16, 197.0000000000000000, -124.6807709998038405 ) ) ;
#12006 = ORIENTED_EDGE ( 'NONE', *, *, #8338, .F. ) ;
#12007 = CARTESIAN_POINT ( 'NONE',  ( -379.3954710152061693, 62.38904131120219176, -128.6202947307455986 ) ) ;
#12008 = CYLINDRICAL_SURFACE ( 'NONE', #4977, 7.500000000000012434 ) ;
#12009 = ORIENTED_EDGE ( 'NONE', *, *, #4965, .F. ) ;
#12010 = CARTESIAN_POINT ( 'NONE',  ( 20.71964524312746647, 180.2041921146487766, -123.3053720114591414 ) ) ;
#12011 = EDGE_LOOP ( 'NONE', ( #1438, #11940, #6503, #11097, #1045 ) ) ;
#12012 = CARTESIAN_POINT ( 'NONE',  ( -1032.644706488202019, 45.21923725197559207, -130.5712005305405228 ) ) ;
#12013 = AXIS2_PLACEMENT_3D ( 'NONE', #8877, #5110, #2209 ) ;
#12014 = DIRECTION ( 'NONE',  ( 0.000000000000000000, 1.000000000000000000, 0.000000000000000000 ) ) ;
#12015 = CARTESIAN_POINT ( 'NONE',  ( 1.249585401188644101E-12, 0.000000000000000000, -6.421356237309494119 ) ) ;
#12016 = CIRCLE ( 'NONE', #3521, 7.500000000000007105 ) ;
#12017 = CARTESIAN_POINT ( 'NONE',  ( -927.6556653799030983, 86.18751778479037284, -95.06748246948041015 ) ) ;
#12018 = CYLINDRICAL_SURFACE ( 'NONE', #7250, 7.500000000000007105 ) ;
#12019 = CARTESIAN_POINT ( 'NONE',  ( 7.500000000000008882, 166.0000000000000000, -124.6807709998038405 ) ) ;
#12020 = EDGE_CURVE ( 'NONE', #11203, #2536, #5425, .T. ) ;
#12021 = ORIENTED_EDGE ( 'NONE', *, *, #2374, .F. ) ;
#12022 = CARTESIAN_POINT ( 'NONE',  ( -818.8285638327207607, 79.00056486031988356, -144.4573442453747703 ) ) ;
#12023 = CARTESIAN_POINT ( 'NONE',  ( 124.6513283658730558, -2.000000000000011102, 123.7119294106446858 ) ) ;
#12024 = DIRECTION ( 'NONE',  ( 0.000000000000000000, -0.8660254037844380415, 0.5000000000000009992 ) ) ;
#12025 = CYLINDRICAL_SURFACE ( 'NONE', #9767, 7.500000000000007105 ) ;
#12026 = EDGE_LOOP ( 'NONE', ( #5938, #11785, #4809, #10959 ) ) ;
#12027 = CARTESIAN_POINT ( 'NONE',  ( -823.5011947277521358, 83.67454157012906535, -154.1077669601579032 ) ) ;
#12028 = CARTESIAN_POINT ( 'NONE',  ( -795.0000000000080718, 82.00000000000049738, -94.48732055948593711 ) ) ;
#12029 = CARTESIAN_POINT ( 'NONE',  ( -795.0000000000043201, 82.00000000000039790, -124.6807709998041105 ) ) ;
#12030 = PRESENTATION_LAYER_ASSIGNMENT (  '', '', ( #5118 ) ) ;
#12031 = CARTESIAN_POINT ( 'NONE',  ( -955.0000000000038654, 82.00000000000036948, -124.6807709998041673 ) ) ;
#12032 = CARTESIAN_POINT ( 'NONE',  ( -126.4213562373094959, -494.9999999999998863, 7.500000000000035527 ) ) ;
#12033 = CARTESIAN_POINT ( 'NONE',  ( 0.8038475772933552088, -5.196152422706605378, 8.999999999999998224 ) ) ;
#12034 = CARTESIAN_POINT ( 'NONE',  ( -827.8143761345638723, 75.63828352384244624, -105.7174308425203861 ) ) ;
#12035 = CARTESIAN_POINT ( 'NONE',  ( -20.72047049683759212, 180.3431580008786170, -123.3086960613613172 ) ) ;
#12036 = EDGE_CURVE ( 'NONE', #10023, #3744, #2468, .T. ) ;
#12037 = ORIENTED_EDGE ( 'NONE', *, *, #10064, .F. ) ;
#12038 = DIRECTION ( 'NONE',  ( 0.000000000000000000, -1.000000000000000000, -7.930164461608263644E-17 ) ) ;
#12039 = EDGE_CURVE ( 'NONE', #5834, #2997, #9112, .T. ) ;
#12040 = DIRECTION ( 'NONE',  ( 0.000000000000000000, 0.000000000000000000, -1.000000000000000000 ) ) ;
#12041 = ADVANCED_FACE ( 'NONE', ( #10047 ), #649, .F. ) ;
#12042 = EDGE_LOOP ( 'NONE', ( #9593, #10156 ) ) ;
#12043 = CARTESIAN_POINT ( 'NONE',  ( -823.8285638327243987, 78.67432280806571043, -264.6807709998050200 ) ) ;
#12044 = CARTESIAN_POINT ( 'NONE',  ( -1021.743962174751232, 119.2557508373789403, -124.6807709998040110 ) ) ;
#12045 = CARTESIAN_POINT ( 'NONE',  ( 9.381075359908434252E-13, 12.00000000000000000, -43.92135623730950300 ) ) ;
#12046 = CYLINDRICAL_SURFACE ( 'NONE', #2337, 7.500000000000020428 ) ;
#12047 = LINE ( 'NONE', #7226, #1887 ) ;
#12048 = CARTESIAN_POINT ( 'NONE',  ( 21.06742223667033542, 181.2647206388604673, -125.9812270727733789 ) ) ;
#12049 = ORIENTED_EDGE ( 'NONE', *, *, #793, .T. ) ;
#12050 = ORIENTED_EDGE ( 'NONE', *, *, #1943, .T. ) ;
#12051 =( REPRESENTATION_RELATIONSHIP ('NONE','NONE', #12149, #4872 ) REPRESENTATION_RELATIONSHIP_WITH_TRANSFORMATION ( #9323 )SHAPE_REPRESENTATION_RELATIONSHIP( ) );
#12052 = LINE ( 'NONE', #6612, #175 ) ;
#12053 = CARTESIAN_POINT ( 'NONE',  ( 6.247927005943220505E-13, 12.00000000000000000, -66.42135623730949590 ) ) ;
#12054 = CARTESIAN_POINT ( 'NONE',  ( -1026.284439350006778, 91.37828661775253636, -154.2940595301281803 ) ) ;
#12055 = CARTESIAN_POINT ( 'NONE',  ( -370.2276204871495224, 107.4109403250190553, -132.4627799267513240 ) ) ;
#12056 = CARTESIAN_POINT ( 'NONE',  ( 0.000000000000000000, -494.9999999999998863, -126.4213562373094959 ) ) ;
#12057 = CARTESIAN_POINT ( 'NONE',  ( 6.899999999999999467, -5.196152422706638241, -9.000000000000001776 ) ) ;
#12058 = CARTESIAN_POINT ( 'NONE',  ( -993.6119331254993767, 96.30709745136249467, -152.5758913445288840 ) ) ;
#12059 = CARTESIAN_POINT ( 'NONE',  ( 27.99999999999999645, -492.9999999999998863, 28.00000000000000000 ) ) ;
#12060 = ORIENTED_EDGE ( 'NONE', *, *, #11988, .F. ) ;
#12061 = DIRECTION ( 'NONE',  ( -0.000000000000000000, 1.000000000000000000, 0.000000000000000000 ) ) ;
#12063 = ADVANCED_FACE ( 'NONE', ( #10171 ), #4062, .T. ) ;
#12062 = CARTESIAN_POINT ( 'NONE',  ( 20.86632180319404029, 178.9255784920988503, -127.0464874675043205 ) ) ;
#12064 = CARTESIAN_POINT ( 'NONE',  ( -381.3712298478259299, 97.88558035699080051, -136.8492573808261170 ) ) ;
#12065 = EDGE_LOOP ( 'NONE', ( #2150, #6708, #8342, #2882, #691, #1907 ) ) ;
#12066 = CARTESIAN_POINT ( 'NONE',  ( -1020.082665824768128, 80.34198733739798115, -154.2940595301280950 ) ) ;
#12067 = CARTESIAN_POINT ( 'NONE',  ( -20.74379340896704704, 180.7482559160401365, -123.4054388444186827 ) ) ;
#12068 = SHAPE_REPRESENTATION ( 'Forming Shoe Axle Center Pin', ( #11957 ), #3662 ) ;
#12069 = EDGE_LOOP ( 'NONE', ( #3389, #3279, #9096, #10217 ) ) ;
#12070 = EDGE_CURVE ( 'NONE', #867, #481, #7638, .T. ) ;
#12071 = VECTOR ( 'NONE', #5591, 1000.000000000000000 ) ;
#12072 = ORIENTED_EDGE ( 'NONE', *, *, #9179, .T. ) ;
#12073 = CARTESIAN_POINT ( 'NONE',  ( -30.00000000000000000, -6.000000000000000000, -30.00000000000000000 ) ) ;
#12074 = CARTESIAN_POINT ( 'NONE',  ( -19.92844181622918143, 182.1616102128938621, -126.3751434161658409 ) ) ;
#12075 = LINE ( 'NONE', #3583, #7984 ) ;
#12076 = ORIENTED_EDGE ( 'NONE', *, *, #2267, .F. ) ;
#12077 = CARTESIAN_POINT ( 'NONE',  ( -381.7589254172675055, 66.96601053460138075, -137.8868535322980904 ) ) ;
#12078 = CARTESIAN_POINT ( 'NONE',  ( 20.00000000000000355, 177.7115707886026144, -124.6807709998038547 ) ) ;
#12079 = MANIFOLD_SOLID_BREP ( 'Fillet9', #2753 ) ;
#12080 = VECTOR ( 'NONE', #844, 1000.000000000000000 ) ;
#12081 = EDGE_CURVE ( 'NONE', #4125, #233, #9187, .T. ) ;
#12082 = ORIENTED_EDGE ( 'NONE', *, *, #2368, .T. ) ;
#12083 = LINE ( 'NONE', #11087, #6418 ) ;
#12084 = AXIS2_PLACEMENT_3D ( 'NONE', #6979, #3149, #1304 ) ;
#12085 = CARTESIAN_POINT ( 'NONE',  ( 0.01899995639452789487, -7.352259170992700987, 5.265513565426383380 ) ) ;
#12086 = CARTESIAN_POINT ( 'NONE',  ( 4.255174644013695128E-15, 25.00000000000002132, -126.4213562373094959 ) ) ;
#12087 = CARTESIAN_POINT ( 'NONE',  ( -955.3297122972882107, 93.84065249268854814, -95.06748246948001224 ) ) ;
#12088 = CARTESIAN_POINT ( 'NONE',  ( -150.0000000000000000, 152.0000000000000000, -126.4213562373084301 ) ) ;
#12089 = CARTESIAN_POINT ( 'NONE',  ( -957.2086549536783195, 47.65337959301152893, -126.6442663926291345 ) ) ;
#12090 = AXIS2_PLACEMENT_3D ( 'NONE', #12088, #4420, #9174 ) ;
#12091 = VECTOR ( 'NONE', #7859, 1000.000000000000000 ) ;
#12092 = ORIENTED_EDGE ( 'NONE', *, *, #11550, .F. ) ;
#12093 = DIRECTION ( 'NONE',  ( -0.000000000000000000, 1.000000000000000000, 7.930164461608263644E-17 ) ) ;
#12094 = CARTESIAN_POINT ( 'NONE',  ( 0.000000000000000000, 0.000000000000000000, 0.000000000000000000 ) ) ;
#12095 = DIRECTION ( 'NONE',  ( 0.000000000000000000, 1.000000000000000000, -0.000000000000000000 ) ) ;
#12096 = CARTESIAN_POINT ( 'NONE',  ( -126.4213562373094959, 0.000000000000000000, -7.499999999999991118 ) ) ;
#12097 = EDGE_LOOP ( 'NONE', ( #2125, #4888, #1383, #11402, #12200, #11652 ) ) ;
#12098 = CARTESIAN_POINT ( 'NONE',  ( -1021.046747802643722, 63.38047825189596551, -103.3307627799639761 ) ) ;
#12099 = LINE ( 'NONE', #10977, #2940 ) ;
#12100 = CARTESIAN_POINT ( 'NONE',  ( -97.49999999999998579, -9.213203435596451385, -126.4213562373088564 ) ) ;
#12101 = CARTESIAN_POINT ( 'NONE',  ( 9.184850993605165694E-16, -492.9999999999998863, -133.9213562373095101 ) ) ;
#12102 = AXIS2_PLACEMENT_3D ( 'NONE', #7500, #9294, #9418 ) ;
#12103 = CARTESIAN_POINT ( 'NONE',  ( -819.8422515189663500, 75.63891865958716210, -105.7172146583290981 ) ) ;
#12104 = CARTESIAN_POINT ( 'NONE',  ( -19.91230007514456446, 178.8584202414884601, -122.8074605759933888 ) ) ;
#12105 = CARTESIAN_POINT ( 'NONE',  ( 2.186774452080127126E-12, 163.9999999999999716, 83.57864376269051832 ) ) ;
#12106 = ORIENTED_EDGE ( 'NONE', *, *, #2029, .T. ) ;
#12107 = ORIENTED_EDGE ( 'NONE', *, *, #2857, .T. ) ;
#12108 = DIRECTION ( 'NONE',  ( 0.000000000000000000, 0.000000000000000000, 1.000000000000000000 ) ) ;
#12109 = ITEM_DEFINED_TRANSFORMATION ( 'NONE', 'NONE', #9193,  #11957 ) ;
#12110 = VERTEX_POINT ( 'NONE', #1834 ) ;
#12111 = DIRECTION ( 'NONE',  ( 0.000000000000000000, 1.000000000000000000, 0.000000000000000000 ) ) ;
#12112 = CARTESIAN_POINT ( 'NONE',  ( -1037.337636019038882, 116.9882293220588991, -124.6807709998043521 ) ) ;
#12113 = CARTESIAN_POINT ( 'NONE',  ( 21.06348120957193260, 180.5399482493916139, -126.3977753017352370 ) ) ;
#12114 = DIRECTION ( 'NONE',  ( 0.000000000000000000, 1.000000000000000000, 0.000000000000000000 ) ) ;
#12115 = DIRECTION ( 'NONE',  ( -1.000000000000000000, 0.000000000000000000, 0.000000000000000000 ) ) ;
#12116 = EDGE_CURVE ( 'NONE', #7316, #1167, #2885, .T. ) ;
#12117 = CARTESIAN_POINT ( 'NONE',  ( 21.06758144644436115, 180.9571029733192233, -126.2348846925512049 ) ) ;
#12118 = EDGE_CURVE ( 'NONE', #1615, #8369, #2806, .T. ) ;
#12119 = VERTEX_POINT ( 'NONE', #584 ) ;
#12120 = AXIS2_PLACEMENT_3D ( 'NONE', #8823, #5540, #11968 ) ;
#12121 = ORIENTED_EDGE ( 'NONE', *, *, #3803, .T. ) ;
#12122 = CARTESIAN_POINT ( 'NONE',  ( -1037.337636019038882, 116.9882293220588991, -124.6807709998043521 ) ) ;
#12123 = CARTESIAN_POINT ( 'NONE',  ( 6.899999999999999467, 0.000000000000000000, 0.000000000000000000 ) ) ;
#12124 = CARTESIAN_POINT ( 'NONE',  ( 4.808665244885994618E-14, 0.000000000000000000, 141.4213562373094817 ) ) ;
#12125 = CARTESIAN_POINT ( 'NONE',  ( -853.3345817150077437, 81.97571759610561060, -154.2940595301280098 ) ) ;
#12126 =( NAMED_UNIT ( * ) PLANE_ANGLE_UNIT ( ) SI_UNIT ( $, .RADIAN. ) );
#12127 = CARTESIAN_POINT ( 'NONE',  ( 20.00000000000000000, 182.6968134406613160, -124.6807709998155076 ) ) ;
#12128 = DIRECTION ( 'NONE',  ( 0.000000000000000000, 0.000000000000000000, 1.000000000000000000 ) ) ;
#12129 = ORIENTED_EDGE ( 'NONE', *, *, #3563, .T. ) ;
#12130 = CARTESIAN_POINT ( 'NONE',  ( 19.00000000000000000, 196.0000000000000000, -124.6807709998038405 ) ) ;
#12131 = AXIS2_PLACEMENT_3D ( 'NONE', #9691, #10440, #7909 ) ;
#12132 = AXIS2_PLACEMENT_3D ( 'NONE', #2723, #617, #7236 ) ;
#12133 = CARTESIAN_POINT ( 'NONE',  ( -384.1738508217867434, 89.73612439111585104, -143.1700354454309547 ) ) ;
#12134 = VERTEX_POINT ( 'NONE', #7803 ) ;
#12135 = CARTESIAN_POINT ( 'NONE',  ( -1047.626240907250804, 63.12837257276900260, -152.5758913445295093 ) ) ;
#12136 = ORIENTED_EDGE ( 'NONE', *, *, #10312, .F. ) ;
#12137 = ADVANCED_FACE ( 'NONE', ( #4950 ), #3268, .F. ) ;
#12138 = ORIENTED_EDGE ( 'NONE', *, *, #5532, .F. ) ;
#12139 = TOROIDAL_SURFACE ( 'NONE', #6794, 19.00000000000000000, 1.000000000000000000 ) ;
#12140 = EDGE_CURVE ( 'NONE', #7569, #8281, #9656, .T. ) ;
#12141 = AXIS2_PLACEMENT_3D ( 'NONE', #11594, #7884, #3226 ) ;
#12142 = AXIS2_PLACEMENT_3D ( 'NONE', #5966, #10603, #1275 ) ;
#12143 = CARTESIAN_POINT ( 'NONE',  ( -827.6116171724385140, 75.38904402457046672, -105.8033998852344695 ) ) ;
#12144 = ORIENTED_EDGE ( 'NONE', *, *, #10971, .T. ) ;
#12145 = CARTESIAN_POINT ( 'NONE',  ( -373.2887456909239745, 65.34136874336766709, -135.8269615355799260 ) ) ;
#12146 = FACE_OUTER_BOUND ( 'NONE', #11004, .T. ) ;
#12147 = EDGE_CURVE ( 'NONE', #8054, #3523, #5043, .T. ) ;
#12148 = DIRECTION ( 'NONE',  ( -1.000000000000000000, 0.000000000000000000, 0.000000000000000000 ) ) ;
#12149 = SHAPE_REPRESENTATION ( 'MAS-313', ( #10783, #305, #7220, #8217, #709, #7625, #2288, #9193, #1697, #8615, #4855, #10186, #6440, #12178, #11193 ), #8811 ) ;
#12150 = AXIS2_PLACEMENT_3D ( 'NONE', #590, #6976, #10746 ) ;
#12151 = CIRCLE ( 'NONE', #5029, 134.9999999999999716 ) ;
#12152 = DIRECTION ( 'NONE',  ( -2.081668171172161734E-17, -4.930380657631307143E-31, 1.000000000000000000 ) ) ;
#12153 = CYLINDRICAL_SURFACE ( 'NONE', #2908, 7.500000000000007105 ) ;
#12154 = CARTESIAN_POINT ( 'NONE',  ( 19.91278132667089906, 178.4073888321768209, -126.5495299892900647 ) ) ;
#12155 = ADVANCED_FACE ( 'NONE', ( #5007 ), #2234, .T. ) ;
#12156 = CARTESIAN_POINT ( 'NONE',  ( -955.9230626098324137, 78.80814421416175719, -95.06748246948052383 ) ) ;
#12157 = DIRECTION ( 'NONE',  ( -1.000000000000000000, -0.000000000000000000, 0.000000000000000000 ) ) ;
#12158 = DIRECTION ( 'NONE',  ( 1.000000000000000000, 0.000000000000000000, 0.000000000000000000 ) ) ;
#12159 = AXIS2_PLACEMENT_3D ( 'NONE', #4896, #8060, #3467 ) ;
#12160 = VECTOR ( 'NONE', #2219, 1000.000000000000000 ) ;
#12161 = ORIENTED_EDGE ( 'NONE', *, *, #9421, .T. ) ;
#12162 = DIRECTION ( 'NONE',  ( 0.000000000000000000, -1.000000000000000000, -7.930164461608263644E-17 ) ) ;
#12163 = DIRECTION ( 'NONE',  ( 0.000000000000000000, 0.000000000000000000, 1.000000000000000000 ) ) ;
#12164 = DIRECTION ( 'NONE',  ( 0.000000000000000000, 0.000000000000000000, 1.000000000000000000 ) ) ;
#12165 = ORIENTED_EDGE ( 'NONE', *, *, #11442, .T. ) ;
#12166 = CARTESIAN_POINT ( 'NONE',  ( -1016.402231264574652, 68.39482517277133411, -99.57582448894554261 ) ) ;
#12167 = CARTESIAN_POINT ( 'NONE',  ( -29.95840947131394572, 180.2041921146317236, -138.2654117679345234 ) ) ;
#12168 = DIRECTION ( 'NONE',  ( 0.000000000000000000, 1.000000000000000000, -0.000000000000000000 ) ) ;
#12169 = DIRECTION ( 'NONE',  ( 0.000000000000000000, 1.000000000000000000, 6.938893903907169213E-16 ) ) ;
#12170 = FACE_OUTER_BOUND ( 'NONE', #5608, .T. ) ;
#12171 = CARTESIAN_POINT ( 'NONE',  ( -819.3334343865096798, 76.46102376401661616, -105.4605772031390813 ) ) ;
#12172 = CARTESIAN_POINT ( 'NONE',  ( -19.97571278480728196, 179.3030001708650332, -123.4829212133057865 ) ) ;
#12173 = CARTESIAN_POINT ( 'NONE',  ( 4.216865464401061553E-15, 168.0000000000000000, -124.6807709998038405 ) ) ;
#12174 = VERTEX_POINT ( 'NONE', #6125 ) ;
#12175 = PRODUCT ( 'Forming Shoe Axle Center Pin', 'Forming Shoe Axle Center Pin', '', ( #8750 ) ) ;
#12176 = CARTESIAN_POINT ( 'NONE',  ( -373.4567406865983799, 67.35621697460008761, -149.6081567629417464 ) ) ;
#12177 = CARTESIAN_POINT ( 'NONE',  ( -373.6140596466332227, 97.17021033344401815, -111.5627346061585570 ) ) ;
#12178 = AXIS2_PLACEMENT_3D ( 'NONE', #3678, #12163, #10354 ) ;
#12179 = ORIENTED_EDGE ( 'NONE', *, *, #3216, .F. ) ;
#12180 = CARTESIAN_POINT ( 'NONE',  ( -904.0006525278403160, 119.6095687608906672, -107.9061927053323160 ) ) ;
#12181 = CIRCLE ( 'NONE', #7634, 69.99999999999998579 ) ;
#12182 = FACE_OUTER_BOUND ( 'NONE', #3654, .T. ) ;
#12183 = CARTESIAN_POINT ( 'NONE',  ( 21.02964448618781645, 181.6776138650130292, -125.1863404894149880 ) ) ;
#12184 = ORIENTED_EDGE ( 'NONE', *, *, #7191, .F. ) ;
#12185 = VERTEX_POINT ( 'NONE', #4152 ) ;
#12186 = CARTESIAN_POINT ( 'NONE',  ( -974.1288507787422759, 124.2142274477005657, -124.6807709998040110 ) ) ;
#12187 = CIRCLE ( 'NONE', #5061, 7.500000000000007105 ) ;
#12188 = LINE ( 'NONE', #11197, #5113 ) ;
#12189 = CARTESIAN_POINT ( 'NONE',  ( 126.4213562373094959, 0.000000000000000000, -6.938893903907228378E-15 ) ) ;
#12190 = CARTESIAN_POINT ( 'NONE',  ( -952.6992609796615170, 94.45070821375009018, -154.2940595301278961 ) ) ;
#12191 = EDGE_CURVE ( 'NONE', #2139, #9220, #2479, .T. ) ;
#12192 = DIRECTION ( 'NONE',  ( 1.000000000000000000, 0.000000000000000000, -0.000000000000000000 ) ) ;
#12193 = CARTESIAN_POINT ( 'NONE',  ( -1046.676250823071769, 92.10743237175765330, -152.5758913445291967 ) ) ;
#12194 = ORIENTED_EDGE ( 'NONE', *, *, #3839, .F. ) ;
#12195 = FACE_OUTER_BOUND ( 'NONE', #809, .T. ) ;
#12196 = ORIENTED_EDGE ( 'NONE', *, *, #3649, .F. ) ;
#12197 = CARTESIAN_POINT ( 'NONE',  ( -795.0000000000071623, 70.44548139156209743, -152.5758913445292535 ) ) ;
#12198 = CIRCLE ( 'NONE', #6854, 7.500000000000007105 ) ;
#12199 = ORIENTED_EDGE ( 'NONE', *, *, #120, .F. ) ;
#12200 = ORIENTED_EDGE ( 'NONE', *, *, #2535, .F. ) ;
#12201 = CARTESIAN_POINT ( 'NONE',  ( -828.0828412852945348, 81.30646073758887837, -144.6692115456662862 ) ) ;
#12202 = CARTESIAN_POINT ( 'NONE',  ( -20.89267889318610472, 181.5262592919334566, -124.1284379062907703 ) ) ;
#12203 = CARTESIAN_POINT ( 'NONE',  ( -372.6621819111771288, 64.05756744580553175, -146.5841632647092183 ) ) ;
#12204 = CARTESIAN_POINT ( 'NONE',  ( 56.53599999999998715, 0.000000000000000000, 0.000000000000000000 ) ) ;
#12205 = EDGE_CURVE ( 'NONE', #11269, #4723, #1616, .T. ) ;
#12206 = FACE_OUTER_BOUND ( 'NONE', #4349, .T. ) ;
#12207 = EDGE_LOOP ( 'NONE', ( #193, #7396, #1223, #1636 ) ) ;
#12208 = AXIS2_PLACEMENT_3D ( 'NONE', #3499, #11054, #6179 ) ;
#12209 = EDGE_CURVE ( 'NONE', #918, #1702, #6185, .T. ) ;
#12210 = CARTESIAN_POINT ( 'NONE',  ( -375.0000000000000000, 81.99999999999995737, -159.6807709998038547 ) ) ;
#12211 = CARTESIAN_POINT ( 'NONE',  ( -28.53314250459844459, 180.2041921146317236, -137.7978499286130898 ) ) ;
#12212 = CARTESIAN_POINT ( 'NONE',  ( -902.6139906877451722, 77.75433758651645633, -96.78565065507919485 ) ) ;
#12213 = CARTESIAN_POINT ( 'NONE',  ( -824.4866663711965202, 83.64159454339613831, -104.7481522953016224 ) ) ;
#12214 = CARTESIAN_POINT ( 'NONE',  ( -854.0902776497797504, 23.28889115110667518, -126.6442663926296603 ) ) ;
#12215 = CARTESIAN_POINT ( 'NONE',  ( -822.5351658412997722, 83.51517767605579934, -144.6233963009600529 ) ) ;
#12216 = ORIENTED_EDGE ( 'NONE', *, *, #9101, .F. ) ;
#12217 = AXIS2_PLACEMENT_3D ( 'NONE', #8849, #11702, #3217 ) ;
#12218 = FACE_BOUND ( 'NONE', #6760, .T. ) ;
#12219 = CARTESIAN_POINT ( 'NONE',  ( 214.0000708641521499, -8.754146129381367759E-15, 23.10407613178388075 ) ) ;
#12220 = ORIENTED_EDGE ( 'NONE', *, *, #11888, .T. ) ;
#12221 = CARTESIAN_POINT ( 'NONE',  ( -1038.506348936316726, 51.71309463382168303, -103.3307627799636350 ) ) ;
#12222 = ADVANCED_FACE ( 'NONE', ( #3452 ), #1489, .F. ) ;
#12223 = DIRECTION ( 'NONE',  ( 0.000000000000000000, 5.522905491341382306E-16, 1.000000000000000000 ) ) ;
#12224 = B_SPLINE_CURVE_WITH_KNOTS ( 'NONE', 3,
 ( #1588, #11913, #5484, #8216, #3433, #7281, #11049, #7219, #5350, #2574, #10597, #9728, #3926, #11714, #7820, #7005, #385, #2312, #3112, #8692, #326, #9672, #142, #1266, #11653, #9609, #3056, #1211, #4112, #6759, #8804, #1091, #202, #8628, #3986, #10716, #7696, #7941, #10777, #4166 ),
 .UNSPECIFIED., .F., .F.,
 ( 4, 2, 2, 2, 2, 2, 2, 2, 2, 2, 2, 2, 2, 2, 2, 2, 2, 2, 2, 4 ),
 ( 6.938893903908117079E-17, 0.0009772159915550746208, 0.001465823987332597837, 0.001954431983110120619, 0.002931647974665001818, 0.003908863966219883017, 0.004886079957774763782, 0.005863295949329645415, 0.006840511940884527048, 0.007817727932439406946, 0.008794943923994288579, 0.009772159915549170212, 0.01026076791132677322, 0.01074937590710437277, 0.01172659189865929950, 0.01270380789021422624, 0.01319241588599166966, 0.01368102388176911655, 0.01465823987332400859, 0.01563545586487890063 ),
 .UNSPECIFIED. ) ;
#12225 = AXIS2_PLACEMENT_3D ( 'NONE', #8483, #1917, #112 ) ;
#12226 = UNCERTAINTY_MEASURE_WITH_UNIT (LENGTH_MEASURE( 1.000000000000000082E-05 ), #8398, 'distance_accuracy_value', 'NONE');
#12227 = VECTOR ( 'NONE', #3711, 1000.000000000000000 ) ;
#12228 = EDGE_CURVE ( 'NONE', #4052, #1330, #4466, .T. ) ;
#12229 = ADVANCED_FACE ( 'NONE', ( #5363 ), #4947, .F. ) ;
#12230 = CARTESIAN_POINT ( 'NONE',  ( -795.0000000000002274, 107.1049510380560719, -107.9061927053326002 ) ) ;
#12231 = CARTESIAN_POINT ( 'NONE',  ( -828.5728621739501705, 77.06309091183271676, -105.2972035265138544 ) ) ;
#12232 = ORIENTED_EDGE ( 'NONE', *, *, #6134, .F. ) ;
#12233 = CARTESIAN_POINT ( 'NONE',  ( 9.371890508914830252E-13, 0.000000000000000000, -28.92135623730948524 ) ) ;
#12234 = CARTESIAN_POINT ( 'NONE',  ( -381.2061940965588747, 98.23031827135795879, -112.9896125472073010 ) ) ;
#12235 = AXIS2_PLACEMENT_3D ( 'NONE', #11001, #11867, #10072 ) ;
#12236 = ORIENTED_EDGE ( 'NONE', *, *, #7002, .F. ) ;
#12237 = CARTESIAN_POINT ( 'NONE',  ( -1024.848917040348397, 116.4131098345821442, -113.1262384684097242 ) ) ;
#12238 = ADVANCED_FACE ( 'NONE', ( #8817 ), #5212, .T. ) ;
#12239 = CARTESIAN_POINT ( 'NONE',  ( -994.8066578865465317, 80.00401887192411721, -154.8742214401228523 ) ) ;
#12240 = NEXT_ASSEMBLY_USAGE_OCCURRENCE ( 'NAUO1', ' ', ' ', #191, #3143, $ ) ;
#12241 = NEXT_ASSEMBLY_USAGE_OCCURRENCE ( 'NAUO2', ' ', ' ', #191, #9935, $ ) ;
#12242 = NEXT_ASSEMBLY_USAGE_OCCURRENCE ( 'NAUO3', ' ', ' ', #191, #7149, $ ) ;
#12243 = NEXT_ASSEMBLY_USAGE_OCCURRENCE ( 'NAUO4', ' ', ' ', #191, #406, $ ) ;
#12244 = NEXT_ASSEMBLY_USAGE_OCCURRENCE ( 'NAUO5', ' ', ' ', #191, #11540, $ ) ;
#12245 = NEXT_ASSEMBLY_USAGE_OCCURRENCE ( 'NAUO6', ' ', ' ', #191, #1872, $ ) ;
#12246 = NEXT_ASSEMBLY_USAGE_OCCURRENCE ( 'NAUO7', ' ', ' ', #191, #9348, $ ) ;
#12247 = NEXT_ASSEMBLY_USAGE_OCCURRENCE ( 'NAUO8', ' ', ' ', #191, #10256, $ ) ;
#12248 = NEXT_ASSEMBLY_USAGE_OCCURRENCE ( 'NAUO9', ' ', ' ', #191, #10256, $ ) ;
#12249 = NEXT_ASSEMBLY_USAGE_OCCURRENCE ( 'NAUO10', ' ', ' ', #191, #406, $ ) ;
#12250 = NEXT_ASSEMBLY_USAGE_OCCURRENCE ( 'NAUO11', ' ', ' ', #191, #3674, $ ) ;
#12251 = NEXT_ASSEMBLY_USAGE_OCCURRENCE ( 'NAUO12', ' ', ' ', #191, #3674, $ ) ;
#12252 = NEXT_ASSEMBLY_USAGE_OCCURRENCE ( 'NAUO13', ' ', ' ', #191, #3674, $ ) ;
#12253 = NEXT_ASSEMBLY_USAGE_OCCURRENCE ( 'NAUO14', ' ', ' ', #191, #3674, $ ) ;
ENDSEC;
END-ISO-10303-21;
